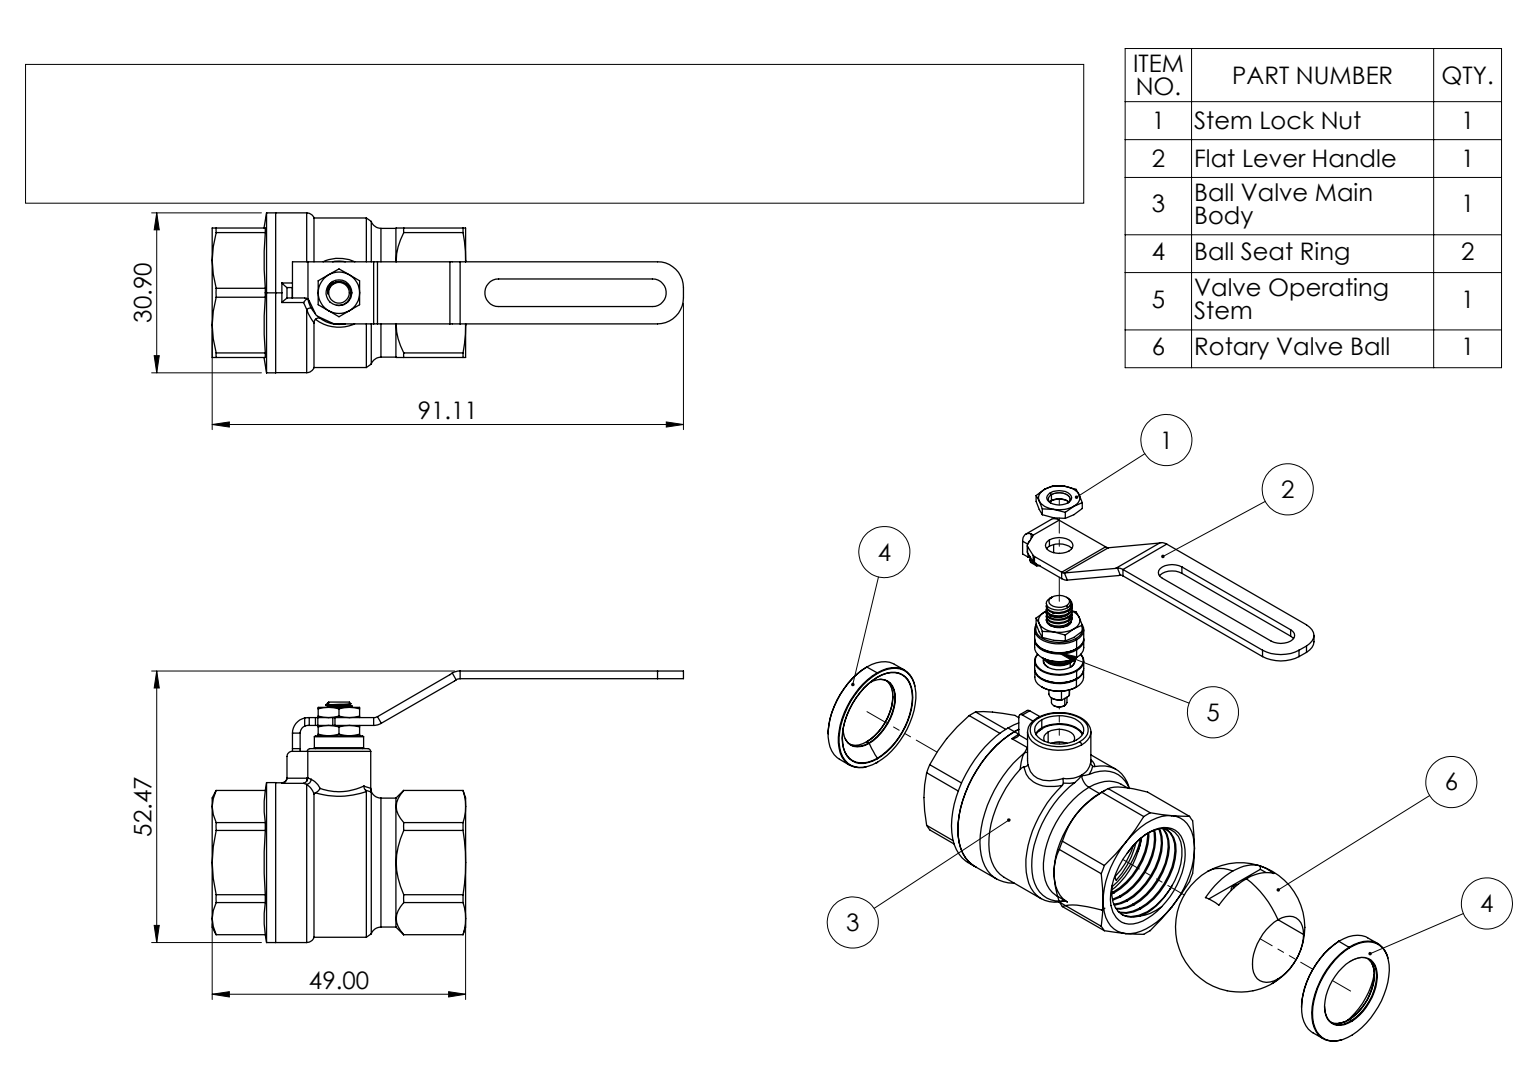
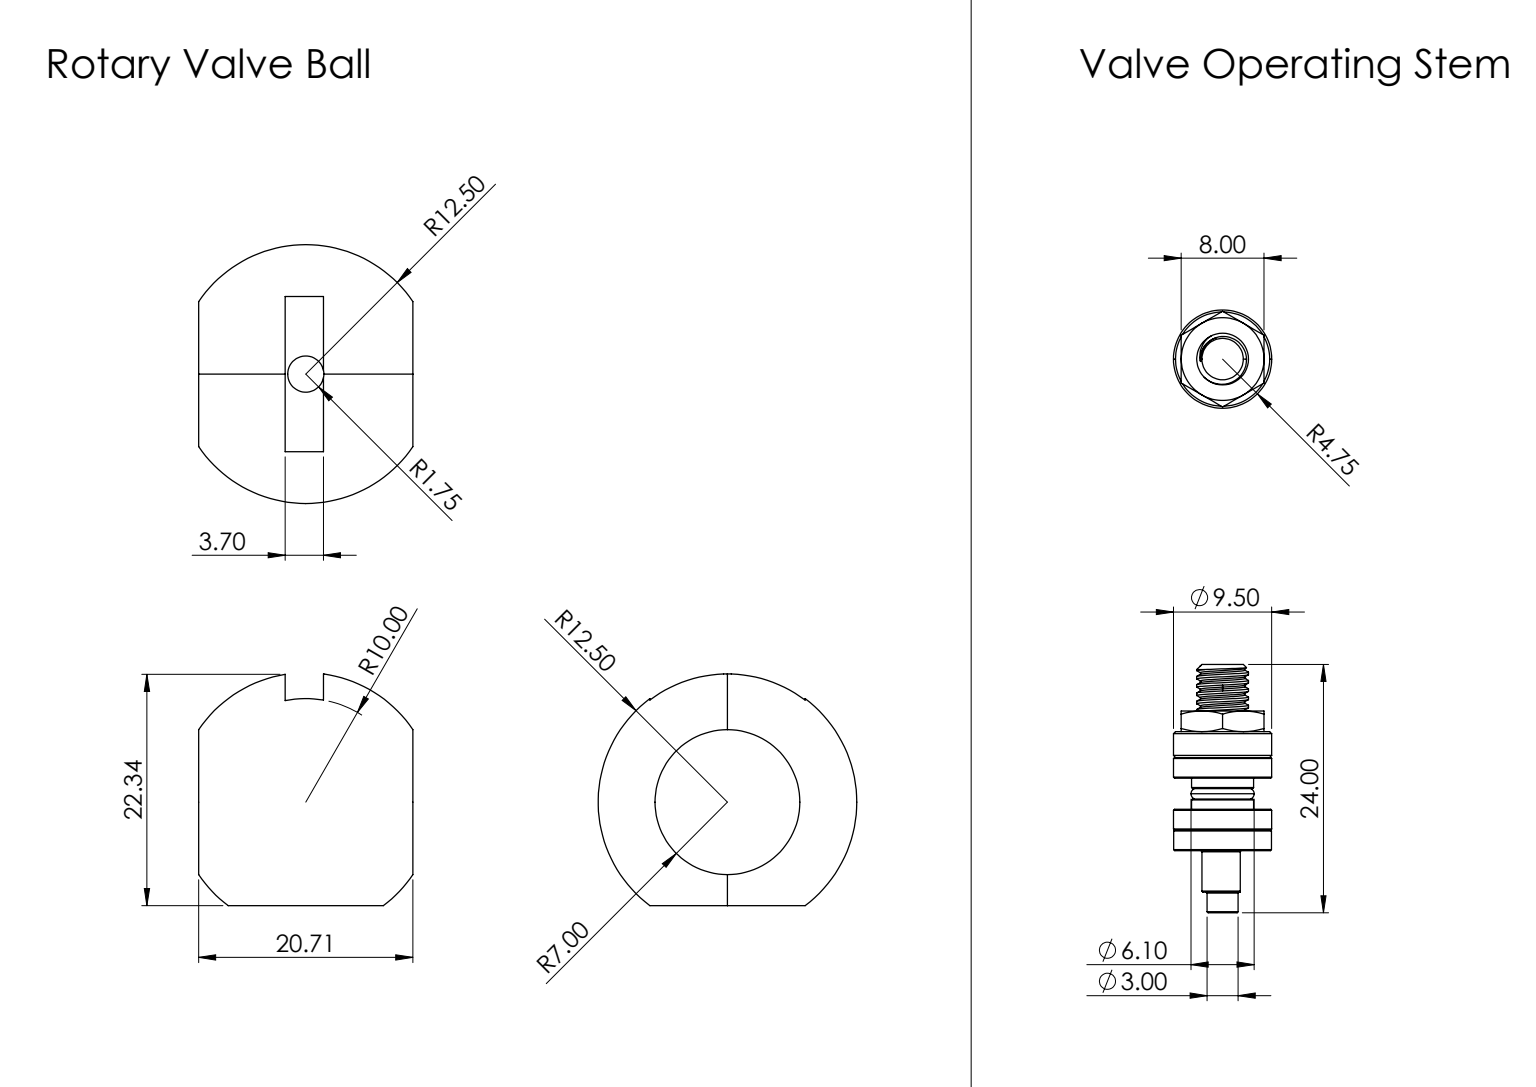
ISO-10303-21;
HEADER;
FILE_DESCRIPTION (('STEP AP214'),
    '1' );
FILE_NAME ('MAS-673',
    '2026-10-09T13:48:35',
    ( '' ),
    ( '' ),
    'SwSTEP 2.0',
    'SolidWorks 2026',
    '' );
FILE_SCHEMA (( 'AUTOMOTIVE_DESIGN' ));
ENDSEC;

DATA;
#1 = VERTEX_POINT ( 'NONE', #550 ) ;
#2 = CARTESIAN_POINT ( 'NONE',  ( -13.11728842303999976, -9.638936811879000643, -0.7309380707209000017 ) ) ;
#3 = CIRCLE ( 'NONE', #13143, 12.50000000000000178 ) ;
#4 = DIRECTION ( 'NONE',  ( 1.000000000000000000, 0.000000000000000000, 0.000000000000000000 ) ) ;
#5 = FACE_OUTER_BOUND ( 'NONE', #6433, .T. ) ;
#6 = EDGE_LOOP ( 'NONE', ( #5081, #3644, #13220, #12725 ) ) ;
#7 = CARTESIAN_POINT ( 'NONE',  ( -10.64042603139669296, 15.44559798911979875, -1.499885078173281761 ) ) ;
#8 = CARTESIAN_POINT ( 'NONE',  ( -1.666640107417000083, 24.57716808515000295, 1.349687702108000043 ) ) ;
#9 = CARTESIAN_POINT ( 'NONE',  ( 14.76827916823049058, 9.002773128276517767, -5.059891690319244795 ) ) ;
#10 = FACE_OUTER_BOUND ( 'NONE', #17299, .T. ) ;
#11 = CARTESIAN_POINT ( 'NONE',  ( 19.46336793902999673, -11.08665823510999893, -1.415474986610000041 ) ) ;
#12 = CARTESIAN_POINT ( 'NONE',  ( -0.8753480283797999695, 29.83343345458000329, -2.192249794771000015 ) ) ;
#13 = CARTESIAN_POINT ( 'NONE',  ( 14.10130024463479792, 4.527370814775449226, 7.815105637936889948 ) ) ;
#14 = CARTESIAN_POINT ( 'NONE',  ( -6.552349917305206439, 15.43140745850629436, -1.524086724148710381 ) ) ;
#15 = DIRECTION ( 'NONE',  ( 0.000000000000000000, 0.000000000000000000, 1.000000000000000000 ) ) ;
#16 = ADVANCED_FACE ( 'NONE', ( #18854 ), #20406, .T. ) ;
#17 = VERTEX_POINT ( 'NONE', #2260 ) ;
#18 = CARTESIAN_POINT ( 'NONE',  ( -2.277512614005948954, 24.29165256314995958, 1.108113113897667867 ) ) ;
#19 = CARTESIAN_POINT ( 'NONE',  ( 24.50000000000000355, -10.15196322910628446, 1.570734485538005432 ) ) ;
#20 = ORIENTED_EDGE ( 'NONE', *, *, #12798, .T. ) ;
#21 = CARTESIAN_POINT ( 'NONE',  ( 11.82354270082560532, -9.054930663370594601, -3.446502399965523988 ) ) ;
#22 = DIRECTION ( 'NONE',  ( -0.4719825803775118955, 0.1835218107899219686, 0.8622947226932178300 ) ) ;
#23 = CARTESIAN_POINT ( 'NONE',  ( 18.51344355829000321, 13.93375672974000068, 0.000000000000000000 ) ) ;
#24 = CARTESIAN_POINT ( 'NONE',  ( 19.10289643275000060, 0.6522580741204999644, 11.12207985314999803 ) ) ;
#25 = AXIS2_PLACEMENT_3D ( 'NONE', #17058, #6275, #4594 ) ;
#26 = CARTESIAN_POINT ( 'NONE',  ( -6.057596641756035183, 16.18429473919449890, 1.000000003976580842 ) ) ;
#27 = CARTESIAN_POINT ( 'NONE',  ( 1.652809762273000027, 26.39462896667000180, -2.096579189799000265 ) ) ;
#28 = EDGE_CURVE ( 'NONE', #3560, #10250, #9953, .T. ) ;
#29 = ORIENTED_EDGE ( 'NONE', *, *, #18417, .F. ) ;
#30 = CARTESIAN_POINT ( 'NONE',  ( -11.32728006584999925, -6.662114061867999482, 13.29187989938000136 ) ) ;
#31 = CARTESIAN_POINT ( 'NONE',  ( 0.000000000000000000, 28.00000000000000000, 0.000000000000000000 ) ) ;
#32 = DIRECTION ( 'NONE',  ( 0.000000000000000000, 0.000000000000000000, -1.000000000000000000 ) ) ;
#33 = ORIENTED_EDGE ( 'NONE', *, *, #678, .T. ) ;
#34 = CARTESIAN_POINT ( 'NONE',  ( -14.44097978627303469, 9.338505494776397242, 8.825220280766517433 ) ) ;
#35 = CARTESIAN_POINT ( 'NONE',  ( 18.85240113949000218, -1.886779804701000041, 10.26112574610000117 ) ) ;
#36 = B_SPLINE_CURVE_WITH_KNOTS ( 'NONE', 3,
 ( #18610, #11347, #22470, #18840, #2244, #6487, #13619, #2487, #661, #2741, #2366, #8067, #8431, #4429, #11583, #6112, #2611, #904 ),
 .UNSPECIFIED., .F., .F.,
 ( 4, 2, 2, 2, 2, 2, 2, 2, 4 ),
 ( 0.000000000000000000, 0.1250000000000000000, 0.2500000000000000000, 0.3750000000000000000, 0.5000000000000000000, 0.6250000000000000000, 0.7500000000000000000, 0.8750000000000000000, 1.000000000000000000 ),
 .UNSPECIFIED. ) ;
#37 = DIRECTION ( 'NONE',  ( 0.7071067811905932254, -0.7071067811824932603, 1.099460906822990477E-07 ) ) ;
#38 = CARTESIAN_POINT ( 'NONE',  ( 15.95305559329677436, -9.354823168593970451, -4.455688050559385438 ) ) ;
#39 = CARTESIAN_POINT ( 'NONE',  ( -16.96748435807999655, 1.976003357569000141, -10.89472041289000082 ) ) ;
#40 = CARTESIAN_POINT ( 'NONE',  ( -1.922540451232000125, 30.13691161737000002, -1.339163193283000153 ) ) ;
#41 = CARTESIAN_POINT ( 'NONE',  ( -14.13294016288999977, 9.260019365940999947, -2.871107829034000414 ) ) ;
#42 = EDGE_CURVE ( 'NONE', #6468, #23190, #12973, .T. ) ;
#43 = CARTESIAN_POINT ( 'NONE',  ( 2.033420667506555812, 29.75788411540394307, 0.7685308260835450600 ) ) ;
#44 = VERTEX_POINT ( 'NONE', #7955 ) ;
#45 = CARTESIAN_POINT ( 'NONE',  ( 0.5694918563224000696, 25.42220128840000015, 2.110394011463000208 ) ) ;
#46 = CARTESIAN_POINT ( 'NONE',  ( 19.50479438917271935, -10.32712268973978276, -1.911112615691448413 ) ) ;
#47 = CARTESIAN_POINT ( 'NONE',  ( -0.9075693228094323661, 23.65758229563746795, -1.957493242368112840 ) ) ;
#48 = ORIENTED_EDGE ( 'NONE', *, *, #10021, .F. ) ;
#49 = CARTESIAN_POINT ( 'NONE',  ( 4.864388344928220143, 14.50529179307395289, -3.789926123251598611 ) ) ;
#50 = EDGE_CURVE ( 'NONE', #3196, #1114, #6484, .T. ) ;
#51 = CARTESIAN_POINT ( 'NONE',  ( 11.28262625730999957, -8.806575700274999363, 0.9184129047361999643 ) ) ;
#52 = ORIENTED_EDGE ( 'NONE', *, *, #12758, .F. ) ;
#53 = B_SPLINE_CURVE_WITH_KNOTS ( 'NONE', 3,
 ( #23724, #16684, #11126, #22035, #20219, #20108, #94, #18511, #3517, #11252 ),
 .UNSPECIFIED., .F., .F.,
 ( 4, 2, 2, 2, 4 ),
 ( 0.000000000000000000, 0.1250000000000000000, 0.2500000000000000000, 0.4999999999999998890, 1.000000000000000000 ),
 .UNSPECIFIED. ) ;
#54 = CARTESIAN_POINT ( 'NONE',  ( -14.25243324638999809, 7.716878364870000340, -11.63397459621999985 ) ) ;
#55 = CARTESIAN_POINT ( 'NONE',  ( -1.999167105995447224, 29.68333333333333357, 1.536366799937292305 ) ) ;
#56 = ORIENTED_EDGE ( 'NONE', *, *, #14846, .T. ) ;
#57 = CARTESIAN_POINT ( 'NONE',  ( -15.49705420454666971, 1.186998013042136924, 9.068966667013654614 ) ) ;
#58 = CARTESIAN_POINT ( 'NONE',  ( 3.983126710162000705, 12.34486698612999866, 2.717232713520998377 ) ) ;
#59 = CARTESIAN_POINT ( 'NONE',  ( 12.00000000000000000, -1.960251216180438627, -9.262521325554040175 ) ) ;
#60 = CARTESIAN_POINT ( 'NONE',  ( -15.96442470609999909, 5.230920372153000208, -8.223195615302000050 ) ) ;
#61 = CARTESIAN_POINT ( 'NONE',  ( 18.86608333333332510, 2.396295210176243362, -8.917180031126768824 ) ) ;
#62 = CARTESIAN_POINT ( 'NONE',  ( -23.39238510356613077, -5.190431350648047726, 9.217397525632280875 ) ) ;
#63 = CARTESIAN_POINT ( 'NONE',  ( 2.213005609277820529, 26.38948373505501266, -0.6062005036607733821 ) ) ;
#64 = FACE_OUTER_BOUND ( 'NONE', #4786, .T. ) ;
#65 = CARTESIAN_POINT ( 'NONE',  ( -5.500092053744999099, 15.58942091952000020, 2.547331119493998042 ) ) ;
#66 = EDGE_CURVE ( 'NONE', #3183, #7147, #11899, .T. ) ;
#67 = CARTESIAN_POINT ( 'NONE',  ( 0.000000000000000000, 29.85000000000000142, 0.000000000000000000 ) ) ;
#68 = ORIENTED_EDGE ( 'NONE', *, *, #2410, .F. ) ;
#69 = ADVANCED_FACE ( 'NONE', ( #11713 ), #19084, .F. ) ;
#70 = CARTESIAN_POINT ( 'NONE',  ( 0.5551539414043799026, 26.26248452079970619, 2.089084675604010233 ) ) ;
#71 = CARTESIAN_POINT ( 'NONE',  ( 13.99789824808406102, 8.658198223038986896, -2.745508126827834516 ) ) ;
#72 = CARTESIAN_POINT ( 'NONE',  ( -22.78638441723432706, -9.917706536484757862, -3.646566398122319530 ) ) ;
#73 = CARTESIAN_POINT ( 'NONE',  ( 1.850881008969999852, 26.55271896306000201, 1.344743706340999934 ) ) ;
#74 = B_SPLINE_CURVE_WITH_KNOTS ( 'NONE', 3,
 ( #8588, #12348, #14154, #1319, #8708, #1438, #3264, #4839, #5196, #6638 ),
 .UNSPECIFIED., .F., .F.,
 ( 4, 2, 2, 2, 4 ),
 ( 0.000000000000000000, 0.1249999999999999722, 0.2499999999999999445, 0.4999999999999998890, 1.000000000000000000 ),
 .UNSPECIFIED. ) ;
#75 = CARTESIAN_POINT ( 'NONE',  ( -2.123790204974259410, 30.86901160495731133, 0.1750885401383986684 ) ) ;
#76 = CARTESIAN_POINT ( 'NONE',  ( 2.570568752299490445, 11.76159806634492000, 4.083892722200570091 ) ) ;
#77 = ORIENTED_EDGE ( 'NONE', *, *, #21426, .F. ) ;
#78 = CARTESIAN_POINT ( 'NONE',  ( -4.424293379393901660, 12.29270965195770771, -1.981197220050498808 ) ) ;
#79 = EDGE_CURVE ( 'NONE', #8805, #20876, #2608, .T. ) ;
#80 = CARTESIAN_POINT ( 'NONE',  ( 24.40278699097224901, 12.15528518867914620, 3.946428472716975833 ) ) ;
#81 = EDGE_CURVE ( 'NONE', #16646, #13895, #14967, .T. ) ;
#82 = DIRECTION ( 'NONE',  ( -1.000000000000000000, 0.000000000000000000, 0.000000000000000000 ) ) ;
#83 = ORIENTED_EDGE ( 'NONE', *, *, #21982, .F. ) ;
#84 = CARTESIAN_POINT ( 'NONE',  ( 0.000000000000000000, 22.00000000000000000, -2.704938617610999654E-14 ) ) ;
#85 = CARTESIAN_POINT ( 'NONE',  ( 15.06487658531000129, -2.993859790429000078, 9.737735315623000432 ) ) ;
#86 = CARTESIAN_POINT ( 'NONE',  ( 18.41753846593428889, 9.434636916628203807, -4.442455713531500372 ) ) ;
#87 = CARTESIAN_POINT ( 'NONE',  ( -1.259047450927242018, 29.16753006952333038, 2.184465970885648201 ) ) ;
#88 = CARTESIAN_POINT ( 'NONE',  ( -1.813125266397999980, 29.53638408233999968, 1.482067624179000065 ) ) ;
#89 = CARTESIAN_POINT ( 'NONE',  ( -5.194121241778000275, 0.000000000000000000, 0.000000000000000000 ) ) ;
#90 = CARTESIAN_POINT ( 'NONE',  ( 0.8889003272348959817, 24.49999999999999289, 2.308449506161659226 ) ) ;
#91 = VECTOR ( 'NONE', #21222, 1000.000000000000114 ) ;
#92 = B_SPLINE_CURVE_WITH_KNOTS ( 'NONE', 3,
 ( #2075, #11646, #16720, #15021, #5828, #18780, #22295, #18555, #5709, #11170 ),
 .UNSPECIFIED., .F., .F.,
 ( 4, 2, 2, 2, 4 ),
 ( 0.000000000000000000, 0.2500000000000000000, 0.5000000000000000000, 0.7500000000000000000, 1.000000000000000000 ),
 .UNSPECIFIED. ) ;
#93 = VERTEX_POINT ( 'NONE', #21155 ) ;
#94 = CARTESIAN_POINT ( 'NONE',  ( -24.37124162822892259, 12.10385983559126544, 4.035505227296849462 ) ) ;
#95 = CARTESIAN_POINT ( 'NONE',  ( 22.24919044816000024, 10.13534249229999951, 5.028067520505000054 ) ) ;
#96 = CARTESIAN_POINT ( 'NONE',  ( -24.02103270219855347, 2.506500440823137055, 9.528970304172808881 ) ) ;
#97 = ORIENTED_EDGE ( 'NONE', *, *, #6382, .F. ) ;
#98 = DIRECTION ( 'NONE',  ( 0.000000000000000000, 1.000000000000000000, 0.000000000000000000 ) ) ;
#99 = CARTESIAN_POINT ( 'NONE',  ( 24.00016455292000117, -9.066063387507998783, 2.014468017461000127 ) ) ;
#100 = CARTESIAN_POINT ( 'NONE',  ( -2.710948798071000088, 11.76207888428000103, 4.122880019904000548 ) ) ;
#101 = CARTESIAN_POINT ( 'NONE',  ( 1.956501129450092469, 29.05944223948321792, -0.9149880855959362513 ) ) ;
#102 = DIRECTION ( 'NONE',  ( 0.000000000000000000, 1.000000000000000000, 0.000000000000000000 ) ) ;
#103 = EDGE_LOOP ( 'NONE', ( #22830, #9902, #9803, #18093 ) ) ;
#104 = CARTESIAN_POINT ( 'NONE',  ( -0.8133812233904295086, 23.73829498092657531, 2.103014135165154563 ) ) ;
#105 = ORIENTED_EDGE ( 'NONE', *, *, #9875, .F. ) ;
#106 = CARTESIAN_POINT ( 'NONE',  ( 0.9654995472831999770, 25.19530436186999722, -2.146034520375999843 ) ) ;
#107 = CARTESIAN_POINT ( 'NONE',  ( 6.643062618671002006, 13.49901315086000686, 0.1224259533632999497 ) ) ;
#108 = CARTESIAN_POINT ( 'NONE',  ( -4.371488211232004595, 13.35998688340998619, 5.531286660341000250 ) ) ;
#109 = AXIS2_PLACEMENT_3D ( 'NONE', #17470, #8390, #618 ) ;
#110 = DIRECTION ( 'NONE',  ( 0.000000000000000000, -1.000000000000000000, 0.000000000000000000 ) ) ;
#111 = CARTESIAN_POINT ( 'NONE',  ( 0.000000000000000000, 19.04999994433000055, -2.949999944334000368 ) ) ;
#112 = CARTESIAN_POINT ( 'NONE',  ( 13.96800158531000058, -3.572926710108999870, -9.509691282521000488 ) ) ;
#113 = CARTESIAN_POINT ( 'NONE',  ( -12.30476703115999904, 8.600742661000001732, -2.211712587549000020 ) ) ;
#114 = CARTESIAN_POINT ( 'NONE',  ( 18.30262625730999915, -5.463569446885998993, 7.195226492777999638 ) ) ;
#115 = DIRECTION ( 'NONE',  ( 1.000000000000000000, 0.000000000000000000, 0.000000000000000000 ) ) ;
#116 = PRODUCT_DEFINITION ( 'UNKNOWN', '', #15975, #23669 ) ;
#117 = ORIENTED_EDGE ( 'NONE', *, *, #18565, .T. ) ;
#118 = CARTESIAN_POINT ( 'NONE',  ( -10.19274265977768579, 15.86535919139761219, -1.103256594710403160 ) ) ;
#119 = B_SPLINE_CURVE_WITH_KNOTS ( 'NONE', 3,
 ( #6295, #17317, #2307, #720, #6416, #11875, #4485, #2421, #8128, #2671, #16960, #10062, #17075, #17447, #15493, #7994, #19128, #22524, #22758, #5931, #9575, #4122, #840, #15126, #13437, #8242, #11756, #15368, #13799, #21198, #11640, #11519, #6177, #359, #18898, #13563, #9694, #473, #7877, #15244, #22636, #20957 ),
 .UNSPECIFIED., .F., .F.,
 ( 4, 2, 1, 2, 2, 2, 1, 2, 2, 2, 2, 2, 2, 2, 2, 1, 2, 2, 2, 1, 2, 2, 4 ),
 ( 0.000000000000000000, 0.06250000000000149880, 0.09375000000000216493, 0.1093750000000024009, 0.1250000000000026368, 0.1875000000000031641, 0.2187500000000033307, 0.2343750000000034139, 0.2500000000000034972, 0.3125000000000032752, 0.3750000000000030531, 0.5000000000000025535, 0.5625000000000022204, 0.6250000000000019984, 0.6875000000000016653, 0.7187500000000015543, 0.7343750000000015543, 0.7500000000000014433, 0.8125000000000007772, 0.8437500000000005551, 0.8593750000000005551, 0.8750000000000004441, 1.000000000000000000 ),
 .UNSPECIFIED. ) ;
#120 = CARTESIAN_POINT ( 'NONE',  ( 2.047900492968999675, 24.12888028435000010, -0.6367493590249000412 ) ) ;
#121 = CARTESIAN_POINT ( 'NONE',  ( 14.61520294907830220, 5.230627013449347551, -8.911388815577064193 ) ) ;
#122 = CARTESIAN_POINT ( 'NONE',  ( -2.000000000000000000, 18.27087121525220681, 0.000000000000000000 ) ) ;
#123 = CARTESIAN_POINT ( 'NONE',  ( 21.99610005449000028, 5.761042396082000749, -9.658588492111000789 ) ) ;
#124 = CARTESIAN_POINT ( 'NONE',  ( 0.4673507188188000261, 29.65618993841000162, -2.509968819301999776 ) ) ;
#125 = CARTESIAN_POINT ( 'NONE',  ( 14.19049813593658982, 1.989872659937805599, 8.829286609355607496 ) ) ;
#126 = CARTESIAN_POINT ( 'NONE',  ( -6.042815832213999983, 16.39253418350000047, -0.9999999878869999526 ) ) ;
#127 = DIRECTION ( 'NONE',  ( 0.000000000000000000, 1.000000000000000000, 0.000000000000000000 ) ) ;
#128 = CARTESIAN_POINT ( 'NONE',  ( 19.17264246499999913, -10.17294749490999983, 5.068503378665999648 ) ) ;
#129 = ORIENTED_EDGE ( 'NONE', *, *, #896, .T. ) ;
#130 = CONICAL_SURFACE ( 'NONE', #12534, 3.049999825846000157, 0.7853981633972997312 ) ;
#131 = CARTESIAN_POINT ( 'NONE',  ( -14.00000000000000000, -15.45000000000000107, 0.000000000000000000 ) ) ;
#132 = EDGE_LOOP ( 'NONE', ( #5049, #12022, #23215, #18123, #9264, #7095, #5187 ) ) ;
#133 = CARTESIAN_POINT ( 'NONE',  ( 0.000000000000000000, 24.50000000000000000, 0.000000000000000000 ) ) ;
#134 = CARTESIAN_POINT ( 'NONE',  ( -2.000000000000000000, 30.00000000000000000, -3.464101615137999968 ) ) ;
#135 = CARTESIAN_POINT ( 'NONE',  ( 14.44500238972999995, 0.2592567778176000370, -11.01108926215000139 ) ) ;
#136 = CARTESIAN_POINT ( 'NONE',  ( -5.833999999999999631, 1.296092693409999996E-14, 0.000000000000000000 ) ) ;
#137 = CARTESIAN_POINT ( 'NONE',  ( 0.5721489135196999865, 28.05212896667000066, -2.607696352436000176 ) ) ;
#138 = ORIENTED_EDGE ( 'NONE', *, *, #17688, .F. ) ;
#139 = ORIENTED_EDGE ( 'NONE', *, *, #19795, .T. ) ;
#140 = CARTESIAN_POINT ( 'NONE',  ( -11.21808363877000048, -14.99030728474000007, -2.625125111862999905 ) ) ;
#141 = CARTESIAN_POINT ( 'NONE',  ( -130.2348000000000070, 19.50000000000000000, -2.000000000000000000 ) ) ;
#142 = CARTESIAN_POINT ( 'NONE',  ( 0.1752525089982897022, 28.25094615491967787, -4.517620070270786492 ) ) ;
#143 = EDGE_CURVE ( 'NONE', #568, #7147, #7639, .T. ) ;
#144 = ORIENTED_EDGE ( 'NONE', *, *, #7334, .F. ) ;
#145 = CARTESIAN_POINT ( 'NONE',  ( -14.48875655809282925, 10.17731420664813413, 7.372365177881404996 ) ) ;
#146 = DIRECTION ( 'NONE',  ( 1.000000000000000000, 0.000000000000000000, 0.000000000000000000 ) ) ;
#147 = CARTESIAN_POINT ( 'NONE',  ( -12.25000000000000000, 1.374666032043000015E-14, 0.000000000000000000 ) ) ;
#148 = CARTESIAN_POINT ( 'NONE',  ( 15.93387064109369433, -9.634484427928969197, -3.804155515456032699 ) ) ;
#149 = CARTESIAN_POINT ( 'NONE',  ( -15.52217783781999927, -9.820682682945999886, -5.027779166633999708 ) ) ;
#150 = CARTESIAN_POINT ( 'NONE',  ( -0.8860051451328000427, 29.33568040543000066, 2.005734967351000098 ) ) ;
#151 = CIRCLE ( 'NONE', #16003, 10.59999999999999964 ) ;
#152 = CIRCLE ( 'NONE', #7126, 1.500000000000001332 ) ;
#153 = CARTESIAN_POINT ( 'NONE',  ( -13.60506528143999994, -10.72046298714999857, -0.8128029906560000351 ) ) ;
#154 = EDGE_CURVE ( 'NONE', #7280, #18990, #3410, .T. ) ;
#155 = CARTESIAN_POINT ( 'NONE',  ( 1.387834333747559601, 29.69250747415173919, 1.655459006554598878 ) ) ;
#156 = ORIENTED_EDGE ( 'NONE', *, *, #22236, .T. ) ;
#157 = CARTESIAN_POINT ( 'NONE',  ( -0.7494000042766999492, 23.97278996295999676, 2.212197947947999843 ) ) ;
#158 = CARTESIAN_POINT ( 'NONE',  ( 21.03695710696093002, -7.396588329481368795, 7.510079579479033818 ) ) ;
#159 = CARTESIAN_POINT ( 'NONE',  ( -18.65919487842199231, 9.743618663561477433, -3.843173192191704501 ) ) ;
#160 = EDGE_LOOP ( 'NONE', ( #4133, #21661, #12489 ) ) ;
#161 = CARTESIAN_POINT ( 'NONE',  ( 0.000000000000000000, 15.00000000000000000, 0.000000000000000000 ) ) ;
#162 = CARTESIAN_POINT ( 'NONE',  ( 1.633245533205915478, 30.34494809611083710, -1.942077254787831109 ) ) ;
#163 = CARTESIAN_POINT ( 'NONE',  ( -23.66121525787396962, 1.340508726618324875, -9.439414443187377657 ) ) ;
#164 = CARTESIAN_POINT ( 'NONE',  ( 17.78062642131000004, 8.824178357484999680, -4.146495103786000058 ) ) ;
#165 = VERTEX_POINT ( 'NONE', #14005 ) ;
#166 = CARTESIAN_POINT ( 'NONE',  ( 0.000000000000000000, 21.87500000000000000, 0.000000000000000000 ) ) ;
#167 = DIRECTION ( 'NONE',  ( 0.000000000000000000, -1.000000000000000000, 0.000000000000000000 ) ) ;
#168 = EDGE_CURVE ( 'NONE', #3985, #21240, #5700, .T. ) ;
#169 = ORIENTED_EDGE ( 'NONE', *, *, #6404, .T. ) ;
#170 = CARTESIAN_POINT ( 'NONE',  ( 23.00512270046333185, 8.092645076355477585, -4.664454223405380517 ) ) ;
#171 = CARTESIAN_POINT ( 'NONE',  ( -4.740217193165002563, 12.61471626404000013, 0.1260612930167998857 ) ) ;
#172 = CARTESIAN_POINT ( 'NONE',  ( -20.26299539000000038, -9.084714414767999457, 1.684552287285000061 ) ) ;
#173 = CARTESIAN_POINT ( 'NONE',  ( 19.11258103379665130, 1.199143088786357669, -9.161748211282004561 ) ) ;
#174 = CARTESIAN_POINT ( 'NONE',  ( -5.483292957314003679, 16.58400099841001918, -3.023963835265001343 ) ) ;
#175 = CARTESIAN_POINT ( 'NONE',  ( -20.53578614557788384, 8.740101311720026800, -5.830131322368356628 ) ) ;
#176 = CARTESIAN_POINT ( 'NONE',  ( 0.000000000000000000, 22.00000000000000000, 0.000000000000000000 ) ) ;
#177 = AXIS2_PLACEMENT_3D ( 'NONE', #2830, #2574, #6813 ) ;
#178 = DIRECTION ( 'NONE',  ( 0.000000000000000000, -1.000000000000000000, 0.000000000000000000 ) ) ;
#179 = CARTESIAN_POINT ( 'NONE',  ( -2.778011591584000239, 28.82750240009999843, -0.7249434865795999494 ) ) ;
#180 = EDGE_CURVE ( 'NONE', #2621, #20551, #276, .T. ) ;
#181 = CARTESIAN_POINT ( 'NONE',  ( 2.147278730106622735, 30.61751797242171591, -0.2331274669797682719 ) ) ;
#182 = EDGE_LOOP ( 'NONE', ( #11413, #48, #13723 ) ) ;
#183 = CARTESIAN_POINT ( 'NONE',  ( 18.24195353945000164, -4.137305632263999833, 8.809128702420998991 ) ) ;
#184 = CARTESIAN_POINT ( 'NONE',  ( 13.84234230361491136, 6.026165916141002832, -6.791106574337510970 ) ) ;
#185 = CARTESIAN_POINT ( 'NONE',  ( -23.10770091748028321, -7.661184619407800156, 7.290997633578977677 ) ) ;
#186 = CARTESIAN_POINT ( 'NONE',  ( 2.048219662131999907, 28.09696440325999944, -1.368576729846999962 ) ) ;
#187 = CARTESIAN_POINT ( 'NONE',  ( -2.123217625947178888, 30.87310701895514597, 0.1259251270839611692 ) ) ;
#188 = CARTESIAN_POINT ( 'NONE',  ( 1.053140587386698135, 11.53014013154227335, 4.696634005027855885 ) ) ;
#189 = ORIENTED_EDGE ( 'NONE', *, *, #3583, .F. ) ;
#190 = EDGE_CURVE ( 'NONE', #10715, #2693, #6863, .T. ) ;
#191 = CARTESIAN_POINT ( 'NONE',  ( -4.144738096053230514, 12.19662818091454426, -2.499798518877363485 ) ) ;
#192 = DIRECTION ( 'NONE',  ( -0.000000000000000000, -1.000000000000000000, -0.000000000000000000 ) ) ;
#193 = DIRECTION ( 'NONE',  ( 0.000000000000000000, 0.000000000000000000, -1.000000000000000000 ) ) ;
#194 = ORIENTED_EDGE ( 'NONE', *, *, #3061, .T. ) ;
#195 = EDGE_CURVE ( 'NONE', #7466, #23288, #17774, .T. ) ;
#196 = EDGE_CURVE ( 'NONE', #21988, #11568, #4015, .T. ) ;
#197 = DIRECTION ( 'NONE',  ( 0.000000000000000000, 1.000000000000000000, 0.000000000000000000 ) ) ;
#198 = CARTESIAN_POINT ( 'NONE',  ( 14.40675158531000122, 9.325397517960999139, -4.058504152148000088 ) ) ;
#199 = AXIS2_PLACEMENT_3D ( 'NONE', #21129, #11572, #17500 ) ;
#200 = CARTESIAN_POINT ( 'NONE',  ( -13.32870921828000021, 6.513713587124000171, -9.206748540250000445 ) ) ;
#201 = DIRECTION ( 'NONE',  ( 1.000000000000000000, 0.000000000000000000, 0.000000000000000000 ) ) ;
#202 = CARTESIAN_POINT ( 'NONE',  ( 16.54676537306000128, 2.042383563461999785, -10.64749026856999947 ) ) ;
#203 = CARTESIAN_POINT ( 'NONE',  ( 8.124934037954998800, 12.44999999999999929, 0.000000000000000000 ) ) ;
#204 = CIRCLE ( 'NONE', #7166, 10.59999999999999964 ) ;
#205 = ORIENTED_EDGE ( 'NONE', *, *, #8949, .F. ) ;
#206 = CARTESIAN_POINT ( 'NONE',  ( 1.709999999999999964, 9.000000000000000000, -7.500000000000000000 ) ) ;
#207 = CARTESIAN_POINT ( 'NONE',  ( 22.95738685678000124, -11.03983583171999960, 2.562588168388999943 ) ) ;
#208 = EDGE_CURVE ( 'NONE', #14474, #22330, #6328, .T. ) ;
#209 = DIRECTION ( 'NONE',  ( -1.000000000000000000, 0.000000000000000000, 0.000000000000000000 ) ) ;
#210 = ORIENTED_EDGE ( 'NONE', *, *, #15775, .T. ) ;
#211 = CARTESIAN_POINT ( 'NONE',  ( -12.48243343204000055, 6.965111533508000718, -5.686492047758000545 ) ) ;
#212 = CARTESIAN_POINT ( 'NONE',  ( 24.50000000000000000, -0.1464674377591403120, 10.48970002016351621 ) ) ;
#213 = CARTESIAN_POINT ( 'NONE',  ( -1.985161156765999468, 11.61875206719000175, 4.524354049390001187 ) ) ;
#214 = CARTESIAN_POINT ( 'NONE',  ( -0.8255343667490313564, 29.25365081292461511, -1.996006782196166229 ) ) ;
#215 = CARTESIAN_POINT ( 'NONE',  ( -21.47533412897999838, 2.576025989571999908, 10.78750342170000032 ) ) ;
#216 = ORIENTED_EDGE ( 'NONE', *, *, #13652, .F. ) ;
#217 = FACE_OUTER_BOUND ( 'NONE', #15939, .T. ) ;
#218 = ORIENTED_EDGE ( 'NONE', *, *, #9354, .F. ) ;
#219 = CARTESIAN_POINT ( 'NONE',  ( 1.782743705658000000, 25.02019945177000082, -1.221832406237000068 ) ) ;
#220 = CARTESIAN_POINT ( 'NONE',  ( 2.434931691670791931, 28.36666666666666359, 0.6543697108981911814 ) ) ;
#221 = FACE_OUTER_BOUND ( 'NONE', #22296, .T. ) ;
#222 = DIRECTION ( 'NONE',  ( -1.000000000000000000, 0.000000000000000000, 0.000000000000000000 ) ) ;
#223 = CIRCLE ( 'NONE', #13763, 3.100000000000000089 ) ;
#224 = CARTESIAN_POINT ( 'NONE',  ( 2.999999956181000016, 17.90000004382000043, -2.609181548331000199E-08 ) ) ;
#225 = FACE_OUTER_BOUND ( 'NONE', #6977, .T. ) ;
#226 = CARTESIAN_POINT ( 'NONE',  ( 17.17537674931000069, -4.906342569036000079, 9.567493125660998743 ) ) ;
#227 = CARTESIAN_POINT ( 'NONE',  ( -16.44889015301999891, 10.17473773424000072, -3.711315847300999948 ) ) ;
#228 = CIRCLE ( 'NONE', #16200, 9.999999999999996447 ) ;
#229 = DIRECTION ( 'NONE',  ( -0.5000000000000169864, 0.8660254037844288266, 0.000000000000000000 ) ) ;
#230 = ORIENTED_EDGE ( 'NONE', *, *, #502, .T. ) ;
#231 = CARTESIAN_POINT ( 'NONE',  ( -10.33759248878110526, 15.67666494535818345, -1.227313276238695794 ) ) ;
#232 = CARTESIAN_POINT ( 'NONE',  ( 0.02135780212313000137, 24.77319310863999746, -2.715970023235000141 ) ) ;
#233 = CARTESIAN_POINT ( 'NONE',  ( 13.88475961963752958, -9.356662177357431887, 4.335039568263141518 ) ) ;
#234 = CARTESIAN_POINT ( 'NONE',  ( 24.50000000000000000, -2.116736914405999759, 10.36413001332999961 ) ) ;
#235 = CARTESIAN_POINT ( 'NONE',  ( 23.83156968415000065, 6.491674009242999865, -9.245099637402999448 ) ) ;
#236 = CARTESIAN_POINT ( 'NONE',  ( 1.879564114486999893, 30.37427879440000211, -1.727888272304000106 ) ) ;
#237 = ADVANCED_FACE ( 'NONE', ( #3364 ), #23073, .T. ) ;
#238 = CARTESIAN_POINT ( 'NONE',  ( 14.09681483843687566, 4.646111251452054169, 7.745166602763706720 ) ) ;
#239 = CARTESIAN_POINT ( 'NONE',  ( 17.04048089729959514, -1.953626282727659813, 10.24653127456325130 ) ) ;
#240 = TOROIDAL_SURFACE ( 'NONE', #10710, 7.200000000000000178, 0.1000000000000000056 ) ;
#241 = FACE_OUTER_BOUND ( 'NONE', #11847, .T. ) ;
#242 = DIRECTION ( 'NONE',  ( 1.000000000000000000, 0.000000000000000000, 0.000000000000000000 ) ) ;
#243 = CARTESIAN_POINT ( 'NONE',  ( 20.33214806635999850, 10.44200582290999968, 4.567853760350999437 ) ) ;
#244 = ORIENTED_EDGE ( 'NONE', *, *, #16225, .T. ) ;
#245 = CARTESIAN_POINT ( 'NONE',  ( 11.78693030657509588, -12.98156941795602215, 2.515258941348812005 ) ) ;
#246 = ORIENTED_EDGE ( 'NONE', *, *, #14119, .T. ) ;
#247 = CARTESIAN_POINT ( 'NONE',  ( -15.91866243917330870, 4.572869834151166657, -7.933744804850305421 ) ) ;
#248 = CARTESIAN_POINT ( 'NONE',  ( 0.000000000000000000, 22.00000000000000000, -4.649999999999999467 ) ) ;
#249 = CARTESIAN_POINT ( 'NONE',  ( 0.1526552725783049125, 24.50000000000000000, 2.395140156181688074 ) ) ;
#250 = CARTESIAN_POINT ( 'NONE',  ( 14.80590418541999931, 10.54075670043000024, -3.228249601621000497 ) ) ;
#251 = CARTESIAN_POINT ( 'NONE',  ( 2.950000000000001954, 24.50000000000000000, 5.832343053588036738E-08 ) ) ;
#252 = CONICAL_SURFACE ( 'NONE', #13040, 1.949955127985000258, 0.7853751480324476786 ) ;
#253 = CARTESIAN_POINT ( 'NONE',  ( 1.182158213329999930, 28.43419433610000269, 2.320116128650000054 ) ) ;
#254 = EDGE_LOOP ( 'NONE', ( #5726, #17524, #14583, #2895 ) ) ;
#255 = ORIENTED_EDGE ( 'NONE', *, *, #14267, .T. ) ;
#256 = CARTESIAN_POINT ( 'NONE',  ( -0.3272492347489394104, 27.25086340285666253, -2.499999999999999112 ) ) ;
#257 = CARTESIAN_POINT ( 'NONE',  ( 1.660953982101407433, 6.978325578095221360, -0.5614028787491848194 ) ) ;
#258 = CARTESIAN_POINT ( 'NONE',  ( 17.75645603379667037, 9.126947370999710429, 1.332864221464923560 ) ) ;
#259 = VERTEX_POINT ( 'NONE', #12444 ) ;
#260 = CARTESIAN_POINT ( 'NONE',  ( 2.000000000000000000, 28.00000000000000000, -3.464101615137999968 ) ) ;
#261 = CARTESIAN_POINT ( 'NONE',  ( 20.92658103379664425, 1.205236576247646685, -9.208299026488377947 ) ) ;
#262 = LINE ( 'NONE', #11311, #3334 ) ;
#263 = CARTESIAN_POINT ( 'NONE',  ( 15.75513086676498808, -10.05562620695802778, 2.464334981930285995 ) ) ;
#264 = CARTESIAN_POINT ( 'NONE',  ( -15.91754618602999827, -1.832079236261000110, 10.89068162177000154 ) ) ;
#265 = CARTESIAN_POINT ( 'NONE',  ( 0.3255751167234999799, 29.40761742610999718, 2.168404648556000236 ) ) ;
#266 = AXIS2_PLACEMENT_3D ( 'NONE', #7745, #20699, #7979 ) ;
#267 = CARTESIAN_POINT ( 'NONE',  ( -19.46889333780000086, -9.261490887677000572, 5.613638565637999456 ) ) ;
#268 = CARTESIAN_POINT ( 'NONE',  ( 1.671545104861497988, 29.71636722689019194, 1.369186538342708204 ) ) ;
#269 = ORIENTED_EDGE ( 'NONE', *, *, #16936, .F. ) ;
#270 = CARTESIAN_POINT ( 'NONE',  ( 1.582682121269000097, 25.73607590313999793, 1.501367095590999901 ) ) ;
#271 = CARTESIAN_POINT ( 'NONE',  ( -2.153985071724999756, 30.83999999999999986, 0.1610847937796999751 ) ) ;
#272 = DIRECTION ( 'NONE',  ( -1.000000000000000000, 0.000000000000000000, 0.000000000000000000 ) ) ;
#273 =( REPRESENTATION_RELATIONSHIP ('NONE','NONE', #13682, #14475 ) REPRESENTATION_RELATIONSHIP_WITH_TRANSFORMATION ( #10971 )SHAPE_REPRESENTATION_RELATIONSHIP( ) );
#274 = EDGE_LOOP ( 'NONE', ( #645, #2365, #19266, #5031 ) ) ;
#275 = EDGE_CURVE ( 'NONE', #9922, #21280, #2869, .T. ) ;
#276 = CIRCLE ( 'NONE', #20030, 12.34057940292999511 ) ;
#277 = CARTESIAN_POINT ( 'NONE',  ( 24.32802197706151048, -3.549421024389301405, 12.49999999999999645 ) ) ;
#278 = FACE_OUTER_BOUND ( 'NONE', #7793, .T. ) ;
#279 = CARTESIAN_POINT ( 'NONE',  ( -23.58077218185689006, 2.644447661185095555, -9.069886164648769622 ) ) ;
#280 = CARTESIAN_POINT ( 'NONE',  ( 12.26981375731000057, 8.958847990383999260, 1.572873132563999965 ) ) ;
#281 = ORIENTED_EDGE ( 'NONE', *, *, #23157, .T. ) ;
#282 = AXIS2_PLACEMENT_3D ( 'NONE', #22952, #17521, #14002 ) ;
#283 = B_SPLINE_CURVE_WITH_KNOTS ( 'NONE', 3,
 ( #2361, #2125, #5763, #13373, #15188, #13148, #20776, #17138, #22466, #7940 ),
 .UNSPECIFIED., .F., .F.,
 ( 4, 2, 2, 2, 4 ),
 ( 0.000000000000000000, 0.2499999999999964473, 0.3749999999999970024, 0.4999999999999975575, 1.000000000000000000 ),
 .UNSPECIFIED. ) ;
#284 = CARTESIAN_POINT ( 'NONE',  ( -4.438477777721789863, 15.42756752407910170, 4.222605013734312962 ) ) ;
#285 = COLOUR_RGB ( '', 0.66274510, 0.83137255, 0.94901961) ;
#286 = CARTESIAN_POINT ( 'NONE',  ( 23.99062354302999722, -13.93375672974000068, 0.8660254037843999608 ) ) ;
#287 = B_SPLINE_SURFACE_WITH_KNOTS ( 'NONE', 3, 3, ( 
 ( #12787, #6851, #14366, #19939, #15924, #16045, #20175, #10379, #14247, #10738, #10621, #21642, #17769, #1171, #3238, #5058, #18007, #1411, #23683, #8804, #16167, #3360, #18130, #7091, #5283, #2110, #1762, #11084, #9619, #9270, #18702, #14817, #9500, #22568, #3935, #14710, #16527, #18818, #22211, #22102, #16753, #11212, #9151, #7435, #16875, #18469, #23914, #7324, #5512, #22329, #7684, #1881, #5625, #20640, #16645, #12890, #280, #20290, #5863, #4051, #5745, #15059, #18351, #3693, #3584, #22453, #51 ),
 ( #13008, #5975, #18592, #20409, #13136, #13247, #11444, #2226, #164, #1997, #20529, #3817, #13357, #17004, #9382, #403, #7801, #7555, #11329, #14934, #15173, #10967, #21248, #23041, #8411, #22801, #11922, #22682, #8040, #1007, #18941, #10222, #17238, #13482, #15649, #639, #19054, #2348, #6463, #15779, #9858, #766, #20884, #4291, #11800, #21120, #19177, #4660, #23168, #12046, #13845, #2586, #19430, #19307, #2840, #9738, #9975, #15289, #2719, #13722, #10101, #15414, #17365, #2467, #8286, #22920, #8166 ),
 ( #17489, #6588, #4531, #7922, #17123, #17614, #6218, #6090, #15534, #4407, #520, #13599, #883, #11680, #20997, #6339, #20758, #4167, #11563, #4900, #8648, #7383, #12288, #17738, #20238, #23287, #14092, #11146, #1143, #18531, #21487, #1260, #16012, #14765, #15895, #21365, #12843, #1940, #9328, #1703, #18413, #19677, #4781, #16702, #23406, #112, #6823, #14219, #3209, #6700, #2960, #3090, #12165, #9209, #5030, #10351, #13972, #19555, #9093, #12414, #10477, #16466, #21614, #10593, #3757, #11028, #1823 ),
 ( #19799, #5460, #17862, #17979, #8537, #23854, #7263, #14655, #22051, #16587, #3642, #23968, #22163, #5574, #12953, #20351, #11508, #7623, #226, #22508, #7862, #5918, #15355, #2526, #7983, #576, #13302, #17180, #6036, #22745, #20472, #20701, #2057, #22625, #460, #13424, #20582, #4110, #5809, #18996, #9681, #18882, #7747, #11627, #9447, #13191, #22273, #20824, #15230, #18650, #9797, #6161, #14999, #20944, #2291, #4234, #4349, #13546, #11740, #19114, #9562, #18759, #2406, #17062, #9918, #17304, #7499 ) ),
 .UNSPECIFIED., .F., .F., .F.,
 ( 4, 4 ),
 ( 4, 1, 1, 1, 1, 1, 1, 1, 1, 1, 1, 1, 1, 1, 1, 1, 1, 1, 1, 1, 1, 1, 1, 1, 1, 1, 1, 1, 1, 1, 1, 1, 1, 1, 1, 1, 1, 1, 1, 1, 1, 1, 1, 1, 1, 1, 1, 1, 1, 1, 1, 1, 1, 1, 1, 1, 1, 1, 1, 1, 1, 1, 1, 1, 4 ),
 ( -0.08331297109794000288, 1.083312971098000066 ),
 ( -0.02000000000000000042, -0.003749999999999999861, 0.01250000000000000069, 0.02875000000000000125, 0.04499999999999999833, 0.06124999999999999889, 0.07749999999999999944, 0.09375000000000000000, 0.1100000000000000006, 0.1262500000000000011, 0.1424999999999999878, 0.1587500000000000022, 0.1749999999999999889, 0.1912500000000000033, 0.2074999999999999900, 0.2237500000000000044, 0.2399999999999999911, 0.2562499999999999778, 0.2725000000000000200, 0.2887500000000000067, 0.3049999999999999933, 0.3212499999999999800, 0.3375000000000000222, 0.3537500000000000089, 0.3699999999999999956, 0.3862499999999999822, 0.4025000000000000244, 0.4187500000000000111, 0.4349999999999999978, 0.4512499999999999845, 0.4675000000000000266, 0.4837500000000000133, 0.5000000000000000000, 0.5162499999999999867, 0.5324999999999999734, 0.5487499999999999600, 0.5649999999999999467, 0.5812500000000000444, 0.5975000000000000311, 0.6137500000000000178, 0.6300000000000000044, 0.6462499999999999911, 0.6624999999999999778, 0.6787499999999999645, 0.6949999999999999512, 0.7112500000000000488, 0.7275000000000000355, 0.7437500000000000222, 0.7600000000000000089, 0.7762499999999999956, 0.7924999999999999822, 0.8087499999999999689, 0.8249999999999999556, 0.8412500000000000533, 0.8575000000000000400, 0.8737500000000000266, 0.8900000000000000133, 0.9062500000000000000, 0.9224999999999999867, 0.9387499999999999734, 0.9549999999999999600, 0.9712499999999999467, 0.9875000000000000444, 1.003749999999999920, 1.020000000000000018 ),
 .UNSPECIFIED. ) ;
#288 = ORIENTED_EDGE ( 'NONE', *, *, #9109, .T. ) ;
#289 = DIRECTION ( 'NONE',  ( 1.000000000000000000, 0.000000000000000000, 0.000000000000000000 ) ) ;
#290 = CARTESIAN_POINT ( 'NONE',  ( -23.29066724161056712, 1.115319073173602238, -9.351742763910808165 ) ) ;
#291 = CARTESIAN_POINT ( 'NONE',  ( -2.623770339515000050, 11.96261007116998876, 4.059183977495999684 ) ) ;
#292 = CARTESIAN_POINT ( 'NONE',  ( -21.81533334470000085, -7.216842995913999914, -6.341849293150000122 ) ) ;
#293 = CARTESIAN_POINT ( 'NONE',  ( -14.46758741243325375, 9.725949910464320780, -8.154098604241012183 ) ) ;
#294 = CARTESIAN_POINT ( 'NONE',  ( -9.481593150953709039E-06, 28.93474093911251899, 2.386566200631719870 ) ) ;
#295 = CARTESIAN_POINT ( 'NONE',  ( -3.025523437588010012, 26.41693820796410463, -2.872015382385962656 ) ) ;
#296 = CARTESIAN_POINT ( 'NONE',  ( -4.750000000000000000, 22.00000000000000000, 0.000000000000000000 ) ) ;
#297 = CARTESIAN_POINT ( 'NONE',  ( 2.155060826509969552, 30.59516583461061145, 0.1486681260086218093 ) ) ;
#298 = ORIENTED_EDGE ( 'NONE', *, *, #14807, .T. ) ;
#299 = CARTESIAN_POINT ( 'NONE',  ( 23.70554140955999856, 3.449944951013000249, 9.831907654028000820 ) ) ;
#300 = CARTESIAN_POINT ( 'NONE',  ( -3.800404330270033437, 13.28692498924355725, -5.638841271150126566 ) ) ;
#301 = FACE_BOUND ( 'NONE', #15644, .T. ) ;
#302 = CONICAL_SURFACE ( 'NONE', #14242, 13.23032192316000000, 1.235249617460683957 ) ;
#303 = ADVANCED_FACE ( 'NONE', ( #21762 ), #7109, .T. ) ;
#304 = CARTESIAN_POINT ( 'NONE',  ( -21.71532941640836256, 6.478598051102530953, 8.484119408269807039 ) ) ;
#305 = CARTESIAN_POINT ( 'NONE',  ( 2.462898805936000191, 27.21946440326000172, 0.04836512055251000058 ) ) ;
#306 = CARTESIAN_POINT ( 'NONE',  ( 24.50000000000000000, 9.974367097857467002, -1.221507673991182219E-15 ) ) ;
#307 = ORIENTED_EDGE ( 'NONE', *, *, #7999, .T. ) ;
#308 = CONICAL_SURFACE ( 'NONE', #4587, 4.649999883068000273, 0.7853981633972997312 ) ;
#309 = CARTESIAN_POINT ( 'NONE',  ( -18.57752051073732247, 7.457970117013407396, -7.338587964615391535 ) ) ;
#310 = CARTESIAN_POINT ( 'NONE',  ( 24.28255857085423131, 12.88093503250115290, 2.689566074712900434 ) ) ;
#311 = VECTOR ( 'NONE', #7009, 1000.000000000000000 ) ;
#312 = FACE_OUTER_BOUND ( 'NONE', #13683, .T. ) ;
#313 = ORIENTED_EDGE ( 'NONE', *, *, #11602, .F. ) ;
#314 = EDGE_CURVE ( 'NONE', #9720, #10966, #3257, .T. ) ;
#315 = CARTESIAN_POINT ( 'NONE',  ( 0.000000000000000000, 24.50000000000000000, 0.000000000000000000 ) ) ;
#316 = CIRCLE ( 'NONE', #702, 0.09999999999999939493 ) ;
#317 = CARTESIAN_POINT ( 'NONE',  ( 18.75768908530999823, -5.059016186635999723, 8.765201904772998986 ) ) ;
#318 = CARTESIAN_POINT ( 'NONE',  ( 23.15628936713000030, 9.265517736846000219, 0.000000000000000000 ) ) ;
#319 = LINE ( 'NONE', #2266, #19710 ) ;
#320 = CARTESIAN_POINT ( 'NONE',  ( 12.61921080085999947, 0.9513980104831999407, -10.33598124465999923 ) ) ;
#321 = DIRECTION ( 'NONE',  ( -0.5000000000000169864, 0.000000000000000000, 0.8660254037844289376 ) ) ;
#322 = ADVANCED_FACE ( 'NONE', ( #21399 ), #12199, .T. ) ;
#323 = DIRECTION ( 'NONE',  ( 0.000000000000000000, -5.996565258237000474E-10, 1.000000000000000000 ) ) ;
#324 = CARTESIAN_POINT ( 'NONE',  ( 23.85409420549000004, -5.578683381639000238, -8.657878734822000766 ) ) ;
#325 = AXIS2_PLACEMENT_3D ( 'NONE', #4418, #15903, #15423 ) ;
#326 = CARTESIAN_POINT ( 'NONE',  ( 23.99062354302999722, 13.93375672974000068, 0.8660254037843999608 ) ) ;
#327 = ORIENTED_EDGE ( 'NONE', *, *, #12498, .T. ) ;
#328 = CARTESIAN_POINT ( 'NONE',  ( 12.10126773346000029, 4.413167110502000945, -7.952200573155999486 ) ) ;
#329 = FACE_OUTER_BOUND ( 'NONE', #10599, .T. ) ;
#330 = CIRCLE ( 'NONE', #15027, 4.000000000000000000 ) ;
#331 = CARTESIAN_POINT ( 'NONE',  ( -4.229412747127002881, 12.27284885278998416, 2.242987681384999377 ) ) ;
#332 = CYLINDRICAL_SURFACE ( 'NONE', #6125, 2.649999999999999911 ) ;
#333 = EDGE_CURVE ( 'NONE', #8084, #19340, #13286, .T. ) ;
#334 = CARTESIAN_POINT ( 'NONE',  ( -19.61694117649999924, -4.574436835851999561, 10.04828037913000216 ) ) ;
#335 = ORIENTED_EDGE ( 'NONE', *, *, #11923, .F. ) ;
#336 = CLOSED_SHELL ( 'NONE', ( #19786, #22741, #8979, #14137, #5705, #10585, #19906, #17710, #15034, #14866, #16344, #2572, #1995, #20352, #20018, #16952, #22187, #19348, #3814, #13211, #2540, #15971, #923, #17120, #9106, #4929, #6763, #19413, #8384, #21247, #11430, #1672, #12020, #13623, #15533, #9283, #9847, #3649, #4205, #7320, #9527, #23189, #20165, #21835, #18823, #16204, #1398 ) ) ;
#337 = CARTESIAN_POINT ( 'NONE',  ( -2.102266727616999731, 23.66000000000000014, 0.4960590750638999569 ) ) ;
#338 = AXIS2_PLACEMENT_3D ( 'NONE', #14363, #14706, #10963 ) ;
#339 = ORIENTED_EDGE ( 'NONE', *, *, #9210, .F. ) ;
#340 = CARTESIAN_POINT ( 'NONE',  ( 5.083787571969999419, 13.95749297742998607, 4.279447512729996461 ) ) ;
#341 = CARTESIAN_POINT ( 'NONE',  ( -1.932944458086000017, 26.02049822780999833, -1.184521108792000010 ) ) ;
#342 = CARTESIAN_POINT ( 'NONE',  ( 16.76949770046334365, -9.101620074973595820, 1.191526229459673347 ) ) ;
#343 = FACE_OUTER_BOUND ( 'NONE', #17510, .T. ) ;
#344 = CARTESIAN_POINT ( 'NONE',  ( 0.000000000000000000, 24.50000000000000000, 0.000000000000000000 ) ) ;
#345 = CIRCLE ( 'NONE', #18552, 7.000000000000000000 ) ;
#346 = EDGE_CURVE ( 'NONE', #1455, #4875, #7182, .T. ) ;
#347 = CARTESIAN_POINT ( 'NONE',  ( -12.61636557635000067, 8.538192823868000048, -4.467067395255999607 ) ) ;
#348 = CONICAL_SURFACE ( 'NONE', #19319, 2.949999944334000368, 0.7853981633972997312 ) ;
#349 = DIRECTION ( 'NONE',  ( 1.000000000000000000, 0.000000000000000000, 0.000000000000000000 ) ) ;
#350 = VECTOR ( 'NONE', #9545, 1000.000000000000000 ) ;
#351 = CARTESIAN_POINT ( 'NONE',  ( -14.38789255204306983, 4.127795921197732198, 12.49979377836116967 ) ) ;
#352 = ORIENTED_EDGE ( 'NONE', *, *, #7893, .F. ) ;
#353 = CARTESIAN_POINT ( 'NONE',  ( 12.50448526289000029, -13.93375672974000068, -0.4329697263849999755 ) ) ;
#354 = CARTESIAN_POINT ( 'NONE',  ( -1.610156619168000125, 25.09339868065000090, 2.187314281954999995 ) ) ;
#355 = CARTESIAN_POINT ( 'NONE',  ( 13.81197141142692253, -8.026017885533216045, 6.503606596646131166 ) ) ;
#356 = CARTESIAN_POINT ( 'NONE',  ( -18.10467920454667023, 2.391415452762288396, -8.898052290273778198 ) ) ;
#357 = CARTESIAN_POINT ( 'NONE',  ( 22.21657238354000086, 10.93369321636999913, 2.658656121609999978 ) ) ;
#358 = CARTESIAN_POINT ( 'NONE',  ( 2.300563072390000130, 28.75630017058999854, 0.5287386102487999784 ) ) ;
#359 = CARTESIAN_POINT ( 'NONE',  ( 11.55284350193499421, 3.530773253024809044, 12.49989659317028057 ) ) ;
#360 = DIRECTION ( 'NONE',  ( 1.000000000000000000, 0.000000000000000000, 0.000000000000000000 ) ) ;
#361 = DIRECTION ( 'NONE',  ( -1.000000000000000000, 0.000000000000000000, 0.000000000000000000 ) ) ;
#362 = EDGE_CURVE ( 'NONE', #11065, #21095, #11524, .T. ) ;
#363 = CARTESIAN_POINT ( 'NONE',  ( 11.78924557931191508, 8.668821331434422461, -9.985146724201950263 ) ) ;
#364 = ORIENTED_EDGE ( 'NONE', *, *, #3722, .T. ) ;
#365 = ADVANCED_FACE ( 'NONE', ( #11334 ), #5191, .T. ) ;
#366 = CARTESIAN_POINT ( 'NONE',  ( 11.59051697473728915, -12.65550321738646211, 3.079847693958680743 ) ) ;
#367 = VERTEX_POINT ( 'NONE', #10972 ) ;
#368 = B_SPLINE_CURVE_WITH_KNOTS ( 'NONE', 3,
 ( #14625, #18275, #16435, #9625, #16880 ),
 .UNSPECIFIED., .F., .F.,
 ( 4, 1, 4 ),
 ( 0.000000000000000000, 0.5000000000000000000, 1.000000000000000000 ),
 .UNSPECIFIED. ) ;
#369 = CARTESIAN_POINT ( 'NONE',  ( -16.25878743917330738, -5.585226852001683895, -7.267873252428181274 ) ) ;
#370 = DIRECTION ( 'NONE',  ( -1.000000000000000000, 0.000000000000000000, 1.562509794170000285E-11 ) ) ;
#371 = PLANE ( 'NONE',  #4207 ) ;
#372 = B_SPLINE_CURVE_WITH_KNOTS ( 'NONE', 3,
 ( #3482, #1297, #5064, #12446, #15814 ),
 .UNSPECIFIED., .F., .F.,
 ( 4, 1, 4 ),
 ( 0.000000000000000000, 0.5000000000000000000, 1.000000000000000000 ),
 .UNSPECIFIED. ) ;
#373 = ORIENTED_EDGE ( 'NONE', *, *, #15908, .F. ) ;
#374 = CIRCLE ( 'NONE', #16631, 0.1000000000000004635 ) ;
#375 = CARTESIAN_POINT ( 'NONE',  ( 16.42996226602999954, 6.392378590226999613, -9.036000841113999371 ) ) ;
#376 = DIRECTION ( 'NONE',  ( 1.000000000000000000, 0.000000000000000000, 0.000000000000000000 ) ) ;
#377 = CARTESIAN_POINT ( 'NONE',  ( -1.864615697012000028, 27.26419433610000098, -2.183184479328999839 ) ) ;
#378 = ADVANCED_FACE ( 'NONE', ( #13011 ), #8274, .F. ) ;
#379 = VERTEX_POINT ( 'NONE', #22107 ) ;
#380 = ORIENTED_EDGE ( 'NONE', *, *, #4764, .F. ) ;
#381 = EDGE_CURVE ( 'NONE', #22357, #8048, #20063, .T. ) ;
#382 = CARTESIAN_POINT ( 'NONE',  ( -14.00000000000000355, -7.644428321857049013, -6.387186174123134386 ) ) ;
#383 = CARTESIAN_POINT ( 'NONE',  ( -10.90524221169000185, 10.44179980742999980, -11.54806271477999857 ) ) ;
#384 = DIRECTION ( 'NONE',  ( 0.000000000000000000, 1.000000000000000000, 0.000000000000000000 ) ) ;
#385 = FACE_OUTER_BOUND ( 'NONE', #7895, .T. ) ;
#386 = VERTEX_POINT ( 'NONE', #18474 ) ;
#387 = CARTESIAN_POINT ( 'NONE',  ( -20.45951251414000183, -9.400720611274998362, 2.131946015016999763 ) ) ;
#388 = CARTESIAN_POINT ( 'NONE',  ( -14.44633158889241287, 12.24656508597993465, 3.788310138426364215 ) ) ;
#389 = CARTESIAN_POINT ( 'NONE',  ( 6.192588632250580538, 13.91017593417528708, 0.8180097329473892120 ) ) ;
#390 = CARTESIAN_POINT ( 'NONE',  ( 15.71064099089155164, -9.557463844202629843, 3.988810051267251300 ) ) ;
#391 = CARTESIAN_POINT ( 'NONE',  ( -14.07687131757000110, -7.628531263931999540, 7.915986703987999640 ) ) ;
#392 = CARTESIAN_POINT ( 'NONE',  ( -2.192033073580000213, 29.19180636409000229, 0.05448754284059999231 ) ) ;
#393 = CARTESIAN_POINT ( 'NONE',  ( -15.83949910911000281, -2.044365629921999883, 10.61848174243000109 ) ) ;
#394 = CARTESIAN_POINT ( 'NONE',  ( 0.5586671089952324198, 29.63706544627255113, 2.086414242290000498 ) ) ;
#395 = ORIENTED_EDGE ( 'NONE', *, *, #16929, .T. ) ;
#396 = CARTESIAN_POINT ( 'NONE',  ( 0.3885665913385000225, 24.40991835864999970, -2.146603527457000116 ) ) ;
#397 = CARTESIAN_POINT ( 'NONE',  ( -4.649999999999999467, 15.00000000000000000, 0.000000000000000000 ) ) ;
#398 = CARTESIAN_POINT ( 'NONE',  ( 24.00016455292000117, 0.000000000000000000, 0.000000000000000000 ) ) ;
#399 = ORIENTED_EDGE ( 'NONE', *, *, #17076, .T. ) ;
#400 = CARTESIAN_POINT ( 'NONE',  ( -0.3006329639645716756, 24.53729095029033758, -2.348355141549282710 ) ) ;
#401 = CARTESIAN_POINT ( 'NONE',  ( -5.600650454439005443, 15.08708793369000034, 2.809640077540999759 ) ) ;
#402 = CARTESIAN_POINT ( 'NONE',  ( 0.000000000000000000, 19.09999999999999787, 0.000000000000000000 ) ) ;
#403 = CARTESIAN_POINT ( 'NONE',  ( 17.01281392131000203, -9.720744103539999514, -0.4165551917177999774 ) ) ;
#404 = ORIENTED_EDGE ( 'NONE', *, *, #21965, .F. ) ;
#405 = CARTESIAN_POINT ( 'NONE',  ( -6.303284018220003837, 15.85635455589998344, -1.061654000538000409 ) ) ;
#406 = DIRECTION ( 'NONE',  ( 0.000000000000000000, 1.000000000000000000, 0.000000000000000000 ) ) ;
#407 = ORIENTED_EDGE ( 'NONE', *, *, #646, .T. ) ;
#408 = CARTESIAN_POINT ( 'NONE',  ( -9.000000000000000000, 19.50000000000000000, -1.000000000000000000 ) ) ;
#409 = CARTESIAN_POINT ( 'NONE',  ( 21.43591666666666740, 2.413791263500860929, 8.981313434221711134 ) ) ;
#410 = CARTESIAN_POINT ( 'NONE',  ( 3.263729719675002361, 12.11073175708999017, 3.451513885400003367 ) ) ;
#411 = LINE ( 'NONE', #6349, #9892 ) ;
#412 = AXIS2_PLACEMENT_3D ( 'NONE', #8961, #23955, #5663 ) ;
#413 = CARTESIAN_POINT ( 'NONE',  ( 12.00000000000000355, -2.493385451254096719, -9.174917364955389232 ) ) ;
#414 = ORIENTED_CLOSED_SHELL ( 'NONE', *, #20462, .F. );
#415 = CARTESIAN_POINT ( 'NONE',  ( 0.000000000000000000, 20.00000000000000000, 0.000000000000000000 ) ) ;
#416 = CARTESIAN_POINT ( 'NONE',  ( -4.749997084077000054, 12.55000000011000161, -4.491085162427999259E-09 ) ) ;
#417 = DIRECTION ( 'NONE',  ( 0.000000000000000000, -0.8660254037844288266, -0.5000000000000169864 ) ) ;
#418 = SURFACE_STYLE_USAGE ( .BOTH. , #3952 ) ;
#419 = CARTESIAN_POINT ( 'NONE',  ( -0.6543697108982035049, 28.06753006952333962, -2.434931691670788823 ) ) ;
#420 = CARTESIAN_POINT ( 'NONE',  ( 2.138730754459550631, 30.58610565302236139, 0.3009471218714359630 ) ) ;
#421 = ORIENTED_EDGE ( 'NONE', *, *, #1138, .T. ) ;
#422 = CARTESIAN_POINT ( 'NONE',  ( 21.14071754283999738, 8.535971018086002005, -4.841000346350999628 ) ) ;
#423 = CARTESIAN_POINT ( 'NONE',  ( 2.342532432829844691, 12.98933061754887497, -6.293791080244014680 ) ) ;
#424 = CARTESIAN_POINT ( 'NONE',  ( 23.75352077758000036, 36.75000000000000000, 6.000000000000000000 ) ) ;
#425 = CARTESIAN_POINT ( 'NONE',  ( -23.56289929282874240, 7.339383936488848903, 7.628101533612420937 ) ) ;
#426 = CARTESIAN_POINT ( 'NONE',  ( 2.425010641684000046, 27.99946440325999930, 0.4330518317348999724 ) ) ;
#427 = CYLINDRICAL_SURFACE ( 'NONE', #12766, 2.999999999999999112 ) ;
#428 = ORIENTED_EDGE ( 'NONE', *, *, #18310, .F. ) ;
#429 = CARTESIAN_POINT ( 'NONE',  ( 0.000000000000000000, 13.04999996922999905, 0.000000000000000000 ) ) ;
#430 = CARTESIAN_POINT ( 'NONE',  ( -2.000000000000000000, 18.89999999999999858, -5.041390465489999878E-11 ) ) ;
#431 = DIRECTION ( 'NONE',  ( 0.000000000000000000, -1.000000000000000000, 0.000000000000000000 ) ) ;
#432 = DIRECTION ( 'NONE',  ( 1.000000000000000000, 0.000000000000000000, 0.000000000000000000 ) ) ;
#433 = ORIENTED_EDGE ( 'NONE', *, *, #18501, .F. ) ;
#434 = FACE_OUTER_BOUND ( 'NONE', #19147, .T. ) ;
#435 = CARTESIAN_POINT ( 'NONE',  ( 14.76225174930999984, 10.68374474379000105, -0.3265774252310000292 ) ) ;
#436 = EDGE_CURVE ( 'NONE', #17309, #8075, #16408, .T. ) ;
#437 = DIRECTION ( 'NONE',  ( 1.000000000000000000, 0.000000000000000000, 0.000000000000000000 ) ) ;
#438 = CARTESIAN_POINT ( 'NONE',  ( -14.25243324638999809, 13.93375672974000068, 0.8660254037843999608 ) ) ;
#439 = CARTESIAN_POINT ( 'NONE',  ( 17.96864037306000128, -10.01334466946000035, -4.258412611471999121 ) ) ;
#440 = CARTESIAN_POINT ( 'NONE',  ( -12.35833339120999952, 6.571898948015506114, -13.37941417155348311 ) ) ;
#441 = CARTESIAN_POINT ( 'NONE',  ( 2.500000000000000000, 29.43419673618999965, 0.000000000000000000 ) ) ;
#442 = CARTESIAN_POINT ( 'NONE',  ( 24.47949698200000057, 5.955140450698999999, -7.767301070824998988 ) ) ;
#443 = VECTOR ( 'NONE', #1417, 1000.000000000000000 ) ;
#444 = CARTESIAN_POINT ( 'NONE',  ( 3.025523437588010012, 29.91693820796410463, 2.872015382385962656 ) ) ;
#445 = ORIENTED_EDGE ( 'NONE', *, *, #2462, .F. ) ;
#446 = LINE ( 'NONE', #20929, #10787 ) ;
#447 = CARTESIAN_POINT ( 'NONE',  ( -2.183184479328999839, 27.17000240009999956, -1.864615697012000028 ) ) ;
#448 = CARTESIAN_POINT ( 'NONE',  ( -4.836833366243003418, 12.42306831226000874, 0.1266535678225001182 ) ) ;
#449 = CARTESIAN_POINT ( 'NONE',  ( 1.973182983453731110, 28.95032424988295361, 0.8828346089906928817 ) ) ;
#450 = ADVANCED_FACE ( 'NONE', ( #1885 ), #12791, .T. ) ;
#451 = CARTESIAN_POINT ( 'NONE',  ( -20.61944845118999936, 1.065297639031000054, -11.01620010679999950 ) ) ;
#452 = ORIENTED_EDGE ( 'NONE', *, *, #7334, .T. ) ;
#453 = DIRECTION ( 'NONE',  ( 0.000000000000000000, 0.000000000000000000, 1.000000000000000000 ) ) ;
#454 = CIRCLE ( 'NONE', #17487, 7.000000000000000000 ) ;
#455 = ORIENTED_EDGE ( 'NONE', *, *, #4994, .F. ) ;
#456 = DIRECTION ( 'NONE',  ( -0.000000000000000000, 1.000000000000000000, 0.000000000000000000 ) ) ;
#457 = CARTESIAN_POINT ( 'NONE',  ( 0.5071914623445000769, 28.61256359724000120, 2.254114612530000006 ) ) ;
#458 = FACE_OUTER_BOUND ( 'NONE', #14382, .T. ) ;
#459 = CARTESIAN_POINT ( 'NONE',  ( -1.433806482797786552, 6.927073644917858708, 1.013309697580697222 ) ) ;
#460 = CARTESIAN_POINT ( 'NONE',  ( 15.42037674930999991, -6.716928621565999791, 8.336789182003000676 ) ) ;
#461 = CARTESIAN_POINT ( 'NONE',  ( -19.53660345378999708, -7.531619525312000185, 7.381236299612999652 ) ) ;
#462 = CARTESIAN_POINT ( 'NONE',  ( 17.20575125731000199, -0.07625726307336000431, -9.225306777752001253 ) ) ;
#463 = CARTESIAN_POINT ( 'NONE',  ( -14.49454881829679920, -0.9069790025675873446, 12.49996723896235906 ) ) ;
#464 = EDGE_CURVE ( 'NONE', #9967, #1877, #3712, .T. ) ;
#465 = ORIENTED_EDGE ( 'NONE', *, *, #22112, .T. ) ;
#466 = FACE_OUTER_BOUND ( 'NONE', #8013, .T. ) ;
#467 = CARTESIAN_POINT ( 'NONE',  ( -2.300703130192000234, 23.53376433680000090, 1.041687086677999918 ) ) ;
#468 = CARTESIAN_POINT ( 'NONE',  ( 13.74204473073353938, -6.236800112200524993, 8.214069492593580435 ) ) ;
#469 = ORIENTED_EDGE ( 'NONE', *, *, #7744, .F. ) ;
#470 = DIRECTION ( 'NONE',  ( 0.000000000000000000, 1.000000000000000000, 0.000000000000000000 ) ) ;
#471 = CARTESIAN_POINT ( 'NONE',  ( 20.52772435074999891, 11.05526862676000022, 1.831395270467999881 ) ) ;
#472 = CARTESIAN_POINT ( 'NONE',  ( 0.2468081092584000213, 28.97172682739000038, -2.347611320519999545 ) ) ;
#473 = CARTESIAN_POINT ( 'NONE',  ( 11.83261479512707659, 4.444106517312727433, 12.50001436053427462 ) ) ;
#474 = CARTESIAN_POINT ( 'NONE',  ( 18.40646359464608395, 10.24499631306186309, 2.163839732140223848 ) ) ;
#475 = CARTESIAN_POINT ( 'NONE',  ( -4.394996721094583059, 13.55525068814215039, 5.016329272847380949 ) ) ;
#476 = CARTESIAN_POINT ( 'NONE',  ( -6.533908178998216520, 15.44339042599172096, 1.502435935679650614 ) ) ;
#477 = EDGE_CURVE ( 'NONE', #16405, #15685, #7206, .T. ) ;
#478 = CARTESIAN_POINT ( 'NONE',  ( -1.259047450927251788, 29.70086340285667603, -2.184465970885643316 ) ) ;
#479 = VERTEX_POINT ( 'NONE', #11804 ) ;
#480 = CIRCLE ( 'NONE', #22909, 2.000000000000000000 ) ;
#481 = CARTESIAN_POINT ( 'NONE',  ( 12.28779254561781720, -13.65788853942738079, 1.343868873886420845 ) ) ;
#482 = ORIENTED_EDGE ( 'NONE', *, *, #4216, .F. ) ;
#483 = PRODUCT ( 'Flat Lever Handle', 'Flat Lever Handle', '', ( #22105 ) ) ;
#484 = CARTESIAN_POINT ( 'NONE',  ( -2.453480368351999896, 24.91848166633000261, 1.213420540718000096 ) ) ;
#486 = CARTESIAN_POINT ( 'NONE',  ( 0.6591105980973780420, 24.04252312545441583, 2.091938566331359883 ) ) ;
#485 = DIRECTION ( 'NONE',  ( 0.000000000000000000, 0.000000000000000000, -1.000000000000000000 ) ) ;
#487 = CARTESIAN_POINT ( 'NONE',  ( 1.640193969998194001, 24.74015355458762144, 1.405240085690787843 ) ) ;
#488 = ORIENTED_EDGE ( 'NONE', *, *, #1439, .F. ) ;
#489 = CARTESIAN_POINT ( 'NONE',  ( -8.000000000000000000, 9.651424765286998664, 0.000000000000000000 ) ) ;
#490 = CARTESIAN_POINT ( 'NONE',  ( -6.161940360818770834, 15.88536285935762038, 1.094220165152027135 ) ) ;
#491 = EDGE_CURVE ( 'NONE', #13012, #9699, #7476, .T. ) ;
#492 = CARTESIAN_POINT ( 'NONE',  ( -1.955724675740084795, 26.26076676662178855, 0.9180910909140133080 ) ) ;
#493 = ORIENTED_EDGE ( 'NONE', *, *, #6761, .F. ) ;
#494 = EDGE_LOOP ( 'NONE', ( #4284, #23458, #17919 ) ) ;
#495 = CARTESIAN_POINT ( 'NONE',  ( -13.99999999999999822, -8.587304723161174991, -5.250545313949140258 ) ) ;
#496 = CARTESIAN_POINT ( 'NONE',  ( -11.00706471169000089, 4.728939151478000369, -14.83327577388999963 ) ) ;
#497 = CARTESIAN_POINT ( 'NONE',  ( 0.4206857880311101749, 6.789717089907916225, -1.702993728068331825 ) ) ;
#498 = CARTESIAN_POINT ( 'NONE',  ( 18.17812270046333367, -0.3397639754939833501, 9.228485993081845251 ) ) ;
#499 = EDGE_CURVE ( 'NONE', #17201, #19976, #8041, .T. ) ;
#500 = ORIENTED_EDGE ( 'NONE', *, *, #19755, .T. ) ;
#501 = CARTESIAN_POINT ( 'NONE',  ( -24.30210239110000003, -9.610041974782999930, 1.174637117329000002 ) ) ;
#502 = EDGE_CURVE ( 'NONE', #22896, #18160, #1313, .T. ) ;
#503 = CARTESIAN_POINT ( 'NONE',  ( -14.48092005499817247, 11.66846015894712707, 4.789644024569511771 ) ) ;
#504 = DIRECTION ( 'NONE',  ( 0.000000000000000000, -1.000000000000000000, 0.000000000000000000 ) ) ;
#505 = CARTESIAN_POINT ( 'NONE',  ( 15.77750233183371265, -10.22258791821789536, 1.644876861122036349 ) ) ;
#506 = CARTESIAN_POINT ( 'NONE',  ( -7.500000000000000000, 22.00000000000000000, 1.000000000000000000 ) ) ;
#507 = CARTESIAN_POINT ( 'NONE',  ( -0.7069816488115999720, 28.78845002726000146, 1.950778716412999936 ) ) ;
#508 = VECTOR ( 'NONE', #15268, 1000.000000000000000 ) ;
#509 = CARTESIAN_POINT ( 'NONE',  ( -13.40193493347000064, -7.644751109369999575, -7.551345029496000727 ) ) ;
#510 = CARTESIAN_POINT ( 'NONE',  ( 0.6475450134985413220, 29.64256677160481956, 2.060670777103924767 ) ) ;
#511 = EDGE_CURVE ( 'NONE', #20864, #19479, #19182, .T. ) ;
#512 = ORIENTED_EDGE ( 'NONE', *, *, #10459, .F. ) ;
#513 = CARTESIAN_POINT ( 'NONE',  ( 0.4803641815392999947, 23.81685268192000038, 2.132454625199999843 ) ) ;
#514 = EDGE_CURVE ( 'NONE', #17995, #19991, #13664, .T. ) ;
#515 = CARTESIAN_POINT ( 'NONE',  ( 0.000000000000000000, 26.50000000000000355, -2.399999999999955502 ) ) ;
#516 = ORIENTED_EDGE ( 'NONE', *, *, #16185, .F. ) ;
#517 = CARTESIAN_POINT ( 'NONE',  ( -22.26176253788000281, -9.242562415387000740, 0.000000000000000000 ) ) ;
#518 = CARTESIAN_POINT ( 'NONE',  ( -4.007822987411000959, 13.30559351321000783, 4.666582981500002170 ) ) ;
#519 = CARTESIAN_POINT ( 'NONE',  ( 0.000000000000000000, 18.00000000000000000, 0.000000000000000000 ) ) ;
#520 = CARTESIAN_POINT ( 'NONE',  ( 17.80706408530999951, 3.725969113535000155, -9.559170675091001712 ) ) ;
#521 = ORIENTED_EDGE ( 'NONE', *, *, #17867, .T. ) ;
#522 = CARTESIAN_POINT ( 'NONE',  ( -6.326119818082997170, 16.13697961988999552, -0.9718497405647000820 ) ) ;
#523 = CARTESIAN_POINT ( 'NONE',  ( 24.00034722001000276, 6.716786535997999685, 12.21137788282999992 ) ) ;
#524 = ORIENTED_EDGE ( 'NONE', *, *, #1140, .F. ) ;
#525 = DIRECTION ( 'NONE',  ( 0.000000000000000000, -0.9998947838056817528, -0.01450590632083973396 ) ) ;
#526 = CARTESIAN_POINT ( 'NONE',  ( 0.000000000000000000, 18.00000000000000000, 0.000000000000000000 ) ) ;
#527 = CARTESIAN_POINT ( 'NONE',  ( 3.924142709797999728, 12.31642185211999241, 2.670936164341001895 ) ) ;
#528 = CARTESIAN_POINT ( 'NONE',  ( -14.00000000000000000, -4.143720316427557115, 9.101378173059835319 ) ) ;
#529 = CARTESIAN_POINT ( 'NONE',  ( 18.34519826651710162, 8.005455623522196973, -6.676223990317056156 ) ) ;
#530 = CARTESIAN_POINT ( 'NONE',  ( 11.99999999999999822, 4.923960526494110646, -7.557474118975338051 ) ) ;
#531 = DIRECTION ( 'NONE',  ( 0.8660254037844288266, 0.5000000000000169864, 0.000000000000000000 ) ) ;
#532 = CARTESIAN_POINT ( 'NONE',  ( 22.24928936712999672, -9.242242329243000043, 0.000000000000000000 ) ) ;
#533 = CARTESIAN_POINT ( 'NONE',  ( -3.821520914465099672, 26.24995697614779644, -2.412446024836691461 ) ) ;
#534 = CARTESIAN_POINT ( 'NONE',  ( 0.000000000000000000, 26.20000000000000284, -4.618802153517000519 ) ) ;
#535 = CARTESIAN_POINT ( 'NONE',  ( -9.000000000000000000, 18.50000000000000000, -5.000000000000000000 ) ) ;
#536 = CARTESIAN_POINT ( 'NONE',  ( 0.3085936222218769731, 30.42196597467193087, 2.139114131937794205 ) ) ;
#537 = EDGE_CURVE ( 'NONE', #23889, #15891, #18705, .T. ) ;
#538 = ORIENTED_EDGE ( 'NONE', *, *, #15854, .F. ) ;
#539 = CARTESIAN_POINT ( 'NONE',  ( 23.65297967911999777, -3.219993159064999944, 9.343258505126000202 ) ) ;
#540 = CARTESIAN_POINT ( 'NONE',  ( 2.127428512114412751, 12.95714030754093926, -6.359730179768805947 ) ) ;
#541 = CARTESIAN_POINT ( 'NONE',  ( -23.65071241290791448, -9.336176072467093690, -1.519767395369341578 ) ) ;
#542 = CARTESIAN_POINT ( 'NONE',  ( -21.15302554097793575, -10.13353536419278278, 2.834801739046542757 ) ) ;
#543 = CARTESIAN_POINT ( 'NONE',  ( 0.4030006639746999686, 26.21114211382000292, 2.256729627096000002 ) ) ;
#544 = DIRECTION ( 'NONE',  ( 0.000000000000000000, -1.000000000000000000, 0.000000000000000000 ) ) ;
#545 = ORIENTED_EDGE ( 'NONE', *, *, #18849, .F. ) ;
#546 = CARTESIAN_POINT ( 'NONE',  ( -19.24739020423550073, -10.46819004694524757, -0.4592041673053260387 ) ) ;
#547 = CARTESIAN_POINT ( 'NONE',  ( -4.000000000000000000, 29.92936170367562809, -1.090349405812125694 ) ) ;
#548 = CIRCLE ( 'NONE', #19927, 0.09999999999999939493 ) ;
#549 = FACE_OUTER_BOUND ( 'NONE', #13999, .T. ) ;
#550 = CARTESIAN_POINT ( 'NONE',  ( -11.04281598264000053, 15.31903517167999951, 1.878299281558999834 ) ) ;
#551 = VERTEX_POINT ( 'NONE', #18822 ) ;
#552 = CARTESIAN_POINT ( 'NONE',  ( 4.000000000000000000, 29.81534065533123723, -1.802053058880664471 ) ) ;
#553 = CARTESIAN_POINT ( 'NONE',  ( 14.87193924930999955, 10.04572779547000039, 3.659788831486999960 ) ) ;
#554 = CARTESIAN_POINT ( 'NONE',  ( -14.14123061016000094, -9.145880708538998149, 6.639339533417000005 ) ) ;
#555 = DIRECTION ( 'NONE',  ( 1.000000000000000000, 0.000000000000000000, 0.000000000000000000 ) ) ;
#556 = CARTESIAN_POINT ( 'NONE',  ( 14.10926537306000128, -9.926075755316000837, 4.188684833930999218 ) ) ;
#557 = CARTESIAN_POINT ( 'NONE',  ( -1.783084334938916715, 30.87983632939971557, -1.147531989998553215 ) ) ;
#558 = DIRECTION ( 'NONE',  ( 0.000000000000000000, 1.000000000000000000, 0.000000000000000000 ) ) ;
#559 = CARTESIAN_POINT ( 'NONE',  ( 24.20819240979999876, 6.272633220716000046, -8.181320936509997921 ) ) ;
#560 = DIRECTION ( 'NONE',  ( 0.000000000000000000, 0.000000000000000000, -1.000000000000000000 ) ) ;
#561 = ORIENTED_EDGE ( 'NONE', *, *, #8358, .F. ) ;
#562 = CARTESIAN_POINT ( 'NONE',  ( 11.84472065189999945, 4.409932236062999777, -7.946371848247000713 ) ) ;
#563 = CARTESIAN_POINT ( 'NONE',  ( -1.394936847711000016, 28.62456776951999871, -2.276308483783000103 ) ) ;
#564 = AXIS2_PLACEMENT_3D ( 'NONE', #17689, #4734, #3281 ) ;
#565 = CARTESIAN_POINT ( 'NONE',  ( 3.627106408426999273, 12.14388422481000518, 3.038632416491001909 ) ) ;
#566 = CARTESIAN_POINT ( 'NONE',  ( 0.2179091018266194058, 28.81668098355705254, 2.159923230666197291 ) ) ;
#567 = CARTESIAN_POINT ( 'NONE',  ( -22.45737845476999794, 0.1502580860940999907, -11.11644552567000055 ) ) ;
#568 = VERTEX_POINT ( 'NONE', #9622 ) ;
#569 = CARTESIAN_POINT ( 'NONE',  ( -4.649999999999999467, 20.10000000000000142, 5.428583055299999740E-09 ) ) ;
#570 = EDGE_LOOP ( 'NONE', ( #6840, #10937, #15562, #10507 ) ) ;
#571 = ADVANCED_FACE ( 'NONE', ( #21002 ), #130, .F. ) ;
#572 = CARTESIAN_POINT ( 'NONE',  ( -24.33938584176924991, 2.815218398139987865, -12.49992678697366166 ) ) ;
#573 = CARTESIAN_POINT ( 'NONE',  ( 2.500000000000000000, 28.40000000000000213, 0.000000000000000000 ) ) ;
#574 = DIRECTION ( 'NONE',  ( 1.000000000000000000, 0.000000000000000000, 0.000000000000000000 ) ) ;
#575 = CARTESIAN_POINT ( 'NONE',  ( -0.3507184568084537046, 6.786897298932621503, 1.714069254809378551 ) ) ;
#576 = CARTESIAN_POINT ( 'NONE',  ( 16.40756424930999913, 8.766565845128001300, -6.190543086277999763 ) ) ;
#577 = CARTESIAN_POINT ( 'NONE',  ( -14.37682859208999986, 9.777980407524001549, -3.031781461267000211 ) ) ;
#578 = CIRCLE ( 'NONE', #21874, 4.625000000000000000 ) ;
#579 = B_SPLINE_CURVE_WITH_KNOTS ( 'NONE', 3,
 ( #6025, #20812, #13412, #20933 ),
 .UNSPECIFIED., .F., .F.,
 ( 4, 4 ),
 ( 0.000000000000000000, 0.6207796204815331231 ),
 .UNSPECIFIED. ) ;
#580 = CARTESIAN_POINT ( 'NONE',  ( 13.91512625730999986, 8.379890869990997970, -3.647050788746000194 ) ) ;
#581 = CARTESIAN_POINT ( 'NONE',  ( -14.48633704289819057, -1.427546401406459831, 12.50000676666411792 ) ) ;
#582 = ORIENTED_EDGE ( 'NONE', *, *, #5142, .F. ) ;
#583 = EDGE_CURVE ( 'NONE', #14220, #9013, #21124, .T. ) ;
#584 = DIRECTION ( 'NONE',  ( 0.000000000000000000, 1.000000000000000000, 0.000000000000000000 ) ) ;
#585 = CARTESIAN_POINT ( 'NONE',  ( 1.924317348631999991, 23.78992879440000152, 1.635700662827000107 ) ) ;
#586 = CARTESIAN_POINT ( 'NONE',  ( 4.418452478372458359, 14.62271791494141837, -4.243679542130283977 ) ) ;
#587 = EDGE_LOOP ( 'NONE', ( #22612, #16356, #15446, #22262 ) ) ;
#588 = CARTESIAN_POINT ( 'NONE',  ( 5.373625923053002573, 13.70222443717999816, -4.580663796643002605 ) ) ;
#589 = DIRECTION ( 'NONE',  ( -0.5000000000000169864, 0.8660254037844288266, 0.000000000000000000 ) ) ;
#590 = CARTESIAN_POINT ( 'NONE',  ( -5.529771451991000397, 1.198997689148999791E-14, 1.310996564781999865E-13 ) ) ;
#591 = CARTESIAN_POINT ( 'NONE',  ( 14.40647870685735832, -4.521102126905931939, 7.829235988601594975 ) ) ;
#592 = CARTESIAN_POINT ( 'NONE',  ( 17.90467403235581045, 0.4259370903896579907, -10.44751290468639660 ) ) ;
#593 = CARTESIAN_POINT ( 'NONE',  ( 2.399999999999999911, 30.00000000000000000, 0.000000000000000000 ) ) ;
#594 = B_SPLINE_CURVE_WITH_KNOTS ( 'NONE', 3,
 ( #15681, #11956, #10132, #23200, #19208, #22833, #547, #673, #21282, #4692 ),
 .UNSPECIFIED., .F., .F.,
 ( 4, 1, 1, 2, 2, 4 ),
 ( 0.000000000000000000, 0.2500000000000001110, 0.3750000000000002776, 0.4375000000000004441, 0.5000000000000005551, 1.000000000000000000 ),
 .UNSPECIFIED. ) ;
#595 =( NAMED_UNIT ( * ) SI_UNIT ( $, .STERADIAN. ) SOLID_ANGLE_UNIT ( ) );
#596 = B_SPLINE_CURVE_WITH_KNOTS ( 'NONE', 3,
 ( #7719, #3848, #14965, #1789 ),
 .UNSPECIFIED., .F., .F.,
 ( 4, 4 ),
 ( 0.000000000000000000, 1.000000000000000000 ),
 .UNSPECIFIED. ) ;
#597 = DIRECTION ( 'NONE',  ( 0.000000000000000000, -1.000000000000000000, 0.000000000000000000 ) ) ;
#598 = ORIENTED_EDGE ( 'NONE', *, *, #22681, .F. ) ;
#599 = AXIS2_PLACEMENT_3D ( 'NONE', #6456, #6583, #635 ) ;
#600 = CARTESIAN_POINT ( 'NONE',  ( 0.000000000000000000, 22.19999999999999574, 0.000000000000000000 ) ) ;
#601 = ORIENTED_EDGE ( 'NONE', *, *, #20949, .F. ) ;
#602 = EDGE_CURVE ( 'NONE', #12251, #21466, #20643, .T. ) ;
#603 = CARTESIAN_POINT ( 'NONE',  ( 2.457689475042000193, 26.10287641827000016, -0.8603483806163000347 ) ) ;
#605 = CARTESIAN_POINT ( 'NONE',  ( -24.50000000000000000, 1.721664336791999924E-14, 0.000000000000000000 ) ) ;
#604 = CARTESIAN_POINT ( 'NONE',  ( -4.270778468753240631, 12.23941797836552148, 2.280178412471628668 ) ) ;
#606 = DIRECTION ( 'NONE',  ( 0.000000000000000000, -1.000000000000000000, 0.000000000000000000 ) ) ;
#607 = CARTESIAN_POINT ( 'NONE',  ( 17.11793655645000101, 6.716980213484000650, 8.821080241391998200 ) ) ;
#608 = CARTESIAN_POINT ( 'NONE',  ( -20.82261444457166988, 6.350348985615495323, 6.750538350822437472 ) ) ;
#609 = CARTESIAN_POINT ( 'NONE',  ( 0.5047246425491000998, 25.99669433610000269, 2.826365205286999860 ) ) ;
#610 = ORIENTED_EDGE ( 'NONE', *, *, #17195, .T. ) ;
#611 = VERTEX_POINT ( 'NONE', #13485 ) ;
#612 = CARTESIAN_POINT ( 'NONE',  ( -14.00000000000000533, -1.777611135496285355, -9.431915595318816514 ) ) ;
#613 = DIRECTION ( 'NONE',  ( -1.000000000000000000, 0.000000000000000000, 0.000000000000000000 ) ) ;
#614 = CARTESIAN_POINT ( 'NONE',  ( -14.48875655809283103, -10.17731420665194797, -7.372365177876170073 ) ) ;
#615 = ORIENTED_EDGE ( 'NONE', *, *, #5201, .F. ) ;
#616 = ADVANCED_FACE ( 'NONE', ( #13361 ), #18050, .F. ) ;
#617 = CARTESIAN_POINT ( 'NONE',  ( -21.73160135699000151, 8.161745128470998978, -6.112658946955999539 ) ) ;
#618 = DIRECTION ( 'NONE',  ( 0.8571428571428744148, 0.000000000000000000, -0.5150787536376840725 ) ) ;
#619 = AXIS2_PLACEMENT_3D ( 'NONE', #16490, #18560, #23879 ) ;
#620 = DIRECTION ( 'NONE',  ( 0.000000000000000000, 1.000000000000000000, 0.000000000000000000 ) ) ;
#621 = CARTESIAN_POINT ( 'NONE',  ( 15.58141692657948596, -6.929050783388004398, 7.685657546460438638 ) ) ;
#622 = AXIS2_PLACEMENT_3D ( 'NONE', #21561, #12361, #8721 ) ;
#623 = CARTESIAN_POINT ( 'NONE',  ( -13.92238738939999898, -10.21016635782999948, -2.519686904309999864 ) ) ;
#624 = DIRECTION ( 'NONE',  ( 0.000000000000000000, 1.000000000000000000, 0.000000000000000000 ) ) ;
#625 = CARTESIAN_POINT ( 'NONE',  ( -21.05048866052816692, -7.545730853300948837, -7.331750953782708358 ) ) ;
#626 = CARTESIAN_POINT ( 'NONE',  ( -14.98621963600000129, -7.639996621784999498, -6.839520901588999280 ) ) ;
#627 = EDGE_CURVE ( 'NONE', #19479, #13618, #15418, .T. ) ;
#628 = CARTESIAN_POINT ( 'NONE',  ( 0.9831177708813756411, 29.66411096424411298, 1.923123576622347120 ) ) ;
#629 = VERTEX_POINT ( 'NONE', #20887 ) ;
#630 = AXIS2_PLACEMENT_3D ( 'NONE', #13866, #4916, #21270 ) ;
#631 = CARTESIAN_POINT ( 'NONE',  ( 1.951212462256999958, 24.89714145383999622, -1.307686770928999875 ) ) ;
#632 = DIRECTION ( 'NONE',  ( 1.000000000000000000, 0.000000000000000000, 0.000000000000000000 ) ) ;
#633 = ORIENTED_EDGE ( 'NONE', *, *, #7921, .T. ) ;
#634 = EDGE_CURVE ( 'NONE', #15280, #17036, #9741, .T. ) ;
#635 = DIRECTION ( 'NONE',  ( 0.000000000000000000, -0.8660254037844288266, 0.5000000000000169864 ) ) ;
#636 = CARTESIAN_POINT ( 'NONE',  ( -0.8571723963710232708, 30.47784972801583692, -2.388390780044352013 ) ) ;
#637 = CARTESIAN_POINT ( 'NONE',  ( 23.41677564524290744, 35.51856778792605240, -6.000000000000000000 ) ) ;
#638 = AXIS2_PLACEMENT_3D ( 'NONE', #10074, #6308, #11771 ) ;
#639 = CARTESIAN_POINT ( 'NONE',  ( 14.81906392131000061, -2.842327771818999871, 9.244929856806999524 ) ) ;
#640 = ORIENTED_EDGE ( 'NONE', *, *, #17076, .F. ) ;
#641 = CYLINDRICAL_SURFACE ( 'NONE', #10623, 1.000000000000000888 ) ;
#642 = B_SPLINE_CURVE_WITH_KNOTS ( 'NONE', 3,
 ( #11380, #22500, #11501, #18876 ),
 .UNSPECIFIED., .F., .F.,
 ( 4, 4 ),
 ( 0.000000000000000000, 1.000000000000000000 ),
 .UNSPECIFIED. ) ;
#643 = CARTESIAN_POINT ( 'NONE',  ( 21.34228936713000024, 9.218966921638999779, 0.000000000000000000 ) ) ;
#644 = CARTESIAN_POINT ( 'NONE',  ( -11.99999999434999864, -6.999999994347000154, -4.083277946868999946E-09 ) ) ;
#645 = ORIENTED_EDGE ( 'NONE', *, *, #11625, .F. ) ;
#646 = EDGE_CURVE ( 'NONE', #14845, #21017, #6325, .T. ) ;
#647 = CARTESIAN_POINT ( 'NONE',  ( -2.206474594537332301, 24.66792226721002734, 0.3902536378939148176 ) ) ;
#648 = CARTESIAN_POINT ( 'NONE',  ( 0.000000000000000000, 19.00000000000000000, 0.000000000000000000 ) ) ;
#649 = CARTESIAN_POINT ( 'NONE',  ( 24.29420393214009977, -1.914062225345805501, 10.44982418693062343 ) ) ;
#650 = DIRECTION ( 'NONE',  ( -1.000000000000000000, 0.000000000000000000, 0.000000000000000000 ) ) ;
#651 = CARTESIAN_POINT ( 'NONE',  ( 17.97914201263965595, -3.906812565131978499, -9.711116240607633898 ) ) ;
#652 = CARTESIAN_POINT ( 'NONE',  ( -23.74465998031000069, 6.216878364870000340, 12.50000000000000000 ) ) ;
#653 = CARTESIAN_POINT ( 'NONE',  ( 7.446152422707000618, 28.20096189432300093, 6.000000000000000000 ) ) ;
#654 = CARTESIAN_POINT ( 'NONE',  ( -4.094404611478998923, 14.04847595166999952, -4.434860849016999396 ) ) ;
#655 = CARTESIAN_POINT ( 'NONE',  ( -0.1784790855350541494, 26.24995697614779644, 4.515757205439222766 ) ) ;
#656 = AXIS2_PLACEMENT_3D ( 'NONE', #17617, #2470, #8045 ) ;
#657 = CARTESIAN_POINT ( 'NONE',  ( 4.829988586904999437, 14.79876397742000194, 3.766541904039999888 ) ) ;
#658 = LINE ( 'NONE', #11344, #22673 ) ;
#659 = CARTESIAN_POINT ( 'NONE',  ( 0.2265999339602371709, 30.41708343718551077, 2.150008283823798383 ) ) ;
#660 = ORIENTED_EDGE ( 'NONE', *, *, #21953, .T. ) ;
#661 = CARTESIAN_POINT ( 'NONE',  ( -17.01462077250666738, 1.192095737878705153, 9.107910416114240348 ) ) ;
#662 = CARTESIAN_POINT ( 'NONE',  ( 24.77691953824000137, -11.46202743651999967, -1.149253455826999781 ) ) ;
#663 = CARTESIAN_POINT ( 'NONE',  ( -2.692449147991668568, 13.04955071611749418, -6.167886193833035158 ) ) ;
#664 = DIRECTION ( 'NONE',  ( 0.000000000000000000, -1.000000000000000000, 0.000000000000000000 ) ) ;
#665 = ADVANCED_FACE ( 'NONE', ( #19057 ), #6222, .T. ) ;
#666 = CARTESIAN_POINT ( 'NONE',  ( -20.53716891550649493, 2.994023850388096708, -10.07133576860161739 ) ) ;
#667 = CARTESIAN_POINT ( 'NONE',  ( 1.525059720042999833, 26.53696440326000072, -1.934529033667000020 ) ) ;
#668 = EDGE_CURVE ( 'NONE', #9155, #14280, #5034, .T. ) ;
#669 = VECTOR ( 'NONE', #2870, 1000.000000000000000 ) ;
#670 = CARTESIAN_POINT ( 'NONE',  ( -3.316026328260925471, 24.63336607546987267, -2.704152903936609231 ) ) ;
#671 = ORIENTED_EDGE ( 'NONE', *, *, #1856, .T. ) ;
#672 = CARTESIAN_POINT ( 'NONE',  ( -17.65644968217466726, -7.789232886291271640, 6.951626983977684304 ) ) ;
#673 = CARTESIAN_POINT ( 'NONE',  ( -4.000000000000000000, 29.87418302490046784, -1.506880184559495239 ) ) ;
#674 = ADVANCED_BREP_SHAPE_REPRESENTATION ( '', ( #9053, #4390 ), #20254 ) ;
#675 = DIRECTION ( 'NONE',  ( -1.000000000000000000, 0.000000000000000000, 0.000000000000000000 ) ) ;
#676 = CARTESIAN_POINT ( 'NONE',  ( 0.000000000000000000, -1.100000000000000089, 0.000000000000000000 ) ) ;
#677 = ORIENTED_EDGE ( 'NONE', *, *, #17568, .T. ) ;
#678 = EDGE_CURVE ( 'NONE', #20171, #3348, #9524, .T. ) ;
#679 = CARTESIAN_POINT ( 'NONE',  ( 17.41195603379666323, 4.591934376281141539, -7.967326209410963145 ) ) ;
#680 = CARTESIAN_POINT ( 'NONE',  ( 15.63975174930999934, -10.61757272617999881, 1.417689269007999853 ) ) ;
#681 = CARTESIAN_POINT ( 'NONE',  ( -24.21952468797000080, 6.266457887630000556, -9.319163484501999051 ) ) ;
#682 = CARTESIAN_POINT ( 'NONE',  ( -17.18818582970000008, -2.107320772642000239, -11.18988855195000021 ) ) ;
#683 = FACE_OUTER_BOUND ( 'NONE', #12131, .T. ) ;
#684 = CARTESIAN_POINT ( 'NONE',  ( 15.05671080085999947, 8.813937669080001314, 7.134837867725000393 ) ) ;
#685 = PLANE ( 'NONE',  #6580 ) ;
#686 = AXIS2_PLACEMENT_3D ( 'NONE', #14903, #16842, #9819 ) ;
#687 = PLANE ( 'NONE',  #16444 ) ;
#688 = CARTESIAN_POINT ( 'NONE',  ( 22.17785865399000045, -8.361523973907999618, -4.965137225652999753 ) ) ;
#689 = PRODUCT_DEFINITION_SHAPE ( 'NONE', 'NONE',  #1482 ) ;
#690 = CARTESIAN_POINT ( 'NONE',  ( 3.999987874060709991, 24.60222989788993431, -1.328900689436832261 ) ) ;
#691 = EDGE_LOOP ( 'NONE', ( #20065, #169, #1554, #10397 ) ) ;
#692 = CARTESIAN_POINT ( 'NONE',  ( 4.829988586904999437, 14.79876397742000016, 3.766541904039999888 ) ) ;
#693 = CARTESIAN_POINT ( 'NONE',  ( 2.052373795670999979, 28.32413313894999973, -1.371352433351999744 ) ) ;
#694 = CARTESIAN_POINT ( 'NONE',  ( 4.543963002250998251, 12.38829681527001370, 1.501761386921000696 ) ) ;
#695 = CARTESIAN_POINT ( 'NONE',  ( 1.836104782222518272, 28.93328551889701927, 1.137863805830989783 ) ) ;
#696 = CARTESIAN_POINT ( 'NONE',  ( -22.95863209211000111, -11.00291023332999885, 1.684196372985999890 ) ) ;
#697 = ORIENTED_EDGE ( 'NONE', *, *, #21937, .T. ) ;
#698 = CARTESIAN_POINT ( 'NONE',  ( -1.600000000000000089, 9.000000000000000000, 0.000000000000000000 ) ) ;
#699 = ORIENTED_EDGE ( 'NONE', *, *, #1410, .F. ) ;
#700 = DIRECTION ( 'NONE',  ( -1.160410170730938003E-09, 2.689653288266210374E-16, -1.000000000000000000 ) ) ;
#701 = CARTESIAN_POINT ( 'NONE',  ( 4.835177208035999818, 0.000000000000000000, 0.000000000000000000 ) ) ;
#702 = AXIS2_PLACEMENT_3D ( 'NONE', #569, #19234, #6518 ) ;
#703 = CARTESIAN_POINT ( 'NONE',  ( 0.1193520287149335557, 6.778461007907296221, 1.747140996228561338 ) ) ;
#704 = CARTESIAN_POINT ( 'NONE',  ( -4.649999849441000421, 19.99999984944626874, 6.648422602291999773E-08 ) ) ;
#705 = CARTESIAN_POINT ( 'NONE',  ( -16.20500172382000059, 9.665285290698001575, -3.525418390172999850 ) ) ;
#706 = CARTESIAN_POINT ( 'NONE',  ( 16.54762625731000014, -6.940875756134999186, 6.051234330564000174 ) ) ;
#707 = CARTESIAN_POINT ( 'NONE',  ( -2.500000000000000000, 27.19999999999999929, 0.000000000000000000 ) ) ;
#708 = AXIS2_PLACEMENT_3D ( 'NONE', #10789, #16573, #20224 ) ;
#709 = VERTEX_POINT ( 'NONE', #2844 ) ;
#710 = CARTESIAN_POINT ( 'NONE',  ( 21.34228936713000024, 9.218966921638999779, 0.000000000000000000 ) ) ;
#711 = CARTESIAN_POINT ( 'NONE',  ( 0.2939441912399000101, 30.67376943012999746, 2.707931486699000079 ) ) ;
#712 = CARTESIAN_POINT ( 'NONE',  ( 0.6575429675851000022, 24.04609325200999947, -2.438473339150000196 ) ) ;
#713 = CIRCLE ( 'NONE', #14639, 1.600000000000000089 ) ;
#714 = CARTESIAN_POINT ( 'NONE',  ( 13.72851662033176545, -5.846715754974600721, 8.501542022457519110 ) ) ;
#715 = AXIS2_PLACEMENT_3D ( 'NONE', #6015, #15457, #201 ) ;
#716 = ORIENTED_EDGE ( 'NONE', *, *, #17809, .F. ) ;
#717 = CARTESIAN_POINT ( 'NONE',  ( 3.941498952056000871, 13.94384724320999602, -4.660668869226999078 ) ) ;
#718 = ADVANCED_FACE ( 'NONE', ( #10105 ), #8276, .T. ) ;
#719 = FACE_OUTER_BOUND ( 'NONE', #14130, .T. ) ;
#720 = CARTESIAN_POINT ( 'NONE',  ( 12.12543434885670557, -5.255139125142729739, 12.50003690309258353 ) ) ;
#721 = CARTESIAN_POINT ( 'NONE',  ( 17.15198968891989395, -5.679900478530641728, 8.758236662128663141 ) ) ;
#722 = PLANE ( 'NONE',  #6401 ) ;
#723 = VECTOR ( 'NONE', #21146, 1000.000000000000000 ) ;
#724 = DIRECTION ( 'NONE',  ( 0.000000000000000000, 1.000000000000000000, 0.000000000000000000 ) ) ;
#725 = CARTESIAN_POINT ( 'NONE',  ( 11.83261479512603032, 8.603276725239243916, -10.09871632138033881 ) ) ;
#726 = EDGE_LOOP ( 'NONE', ( #11462, #19788, #12642, #19276 ) ) ;
#727 = CARTESIAN_POINT ( 'NONE',  ( 11.43887872962553054, -12.36312605252038033, 3.586317572276362942 ) ) ;
#728 = ORIENTED_EDGE ( 'NONE', *, *, #1649, .T. ) ;
#729 = VECTOR ( 'NONE', #20922, 1000.000000000000000 ) ;
#730 = DIRECTION ( 'NONE',  ( 0.000000000000000000, 0.4098987730065234425, -0.9121310190360518710 ) ) ;
#732 = DIRECTION ( 'NONE',  ( 0.000000000000000000, -1.000000000000000000, 1.361873576874000145E-14 ) ) ;
#731 = CARTESIAN_POINT ( 'NONE',  ( -0.2205931549149543758, 11.48217017896666015, 4.812798745242788279 ) ) ;
#733 = CARTESIAN_POINT ( 'NONE',  ( 8.124934037954998800, 0.000000000000000000, 0.000000000000000000 ) ) ;
#734 = AXIS2_PLACEMENT_3D ( 'NONE', #10520, #4708, #10636 ) ;
#735 = CARTESIAN_POINT ( 'NONE',  ( 1.699986466736000068, 9.100024030970999434, -1.053574575520999757 ) ) ;
#736 = DIRECTION ( 'NONE',  ( 0.8660254037844288266, 0.5000000000000169864, 0.000000000000000000 ) ) ;
#737 = CARTESIAN_POINT ( 'NONE',  ( 2.844001364980000002, 26.19169433609999942, -0.3933730402103999824 ) ) ;
#738 = EDGE_LOOP ( 'NONE', ( #3127, #3699, #18368, #8559 ) ) ;
#739 = ORIENTED_EDGE ( 'NONE', *, *, #9983, .F. ) ;
#740 = CARTESIAN_POINT ( 'NONE',  ( -13.99999999999999645, -4.994886009442610408, -8.411685227471448201 ) ) ;
#741 = TOROIDAL_SURFACE ( 'NONE', #11184, 16.43375672870000059, 1.000000000000000000 ) ;
#742 = DIRECTION ( 'NONE',  ( 0.000000000000000000, 1.000000000000000000, 0.000000000000000000 ) ) ;
#743 = CARTESIAN_POINT ( 'NONE',  ( -24.24003052283108062, -9.030352382187791349, -9.358674018439064213 ) ) ;
#744 = VERTEX_POINT ( 'NONE', #12419 ) ;
#745 = CARTESIAN_POINT ( 'NONE',  ( -21.31634619217999926, 9.651037232871999549, -0.4757113999236000090 ) ) ;
#746 = CARTESIAN_POINT ( 'NONE',  ( -18.99854661335000117, -6.966878364870000340, 12.06698729810999993 ) ) ;
#747 = FACE_OUTER_BOUND ( 'NONE', #13182, .T. ) ;
#748 = CARTESIAN_POINT ( 'NONE',  ( 15.86493638691169750, -10.25014446212039587, -1.494075193881422514 ) ) ;
#749 = CARTESIAN_POINT ( 'NONE',  ( -17.80271749694000150, -11.00587167721000093, 1.406230294539999814 ) ) ;
#750 = CIRCLE ( 'NONE', #8500, 1.500000000000000000 ) ;
#751 = EDGE_CURVE ( 'NONE', #9876, #8499, #3436, .T. ) ;
#752 = CARTESIAN_POINT ( 'NONE',  ( 0.3930574723085999977, 29.80062481890999848, -2.323201669609999964 ) ) ;
#753 = CARTESIAN_POINT ( 'NONE',  ( -20.92181303178861285, -3.650616230715998611, -9.863665015250019152 ) ) ;
#754 = DIRECTION ( 'NONE',  ( 0.000000000000000000, 1.000000000000000000, 0.000000000000000000 ) ) ;
#755 = CARTESIAN_POINT ( 'NONE',  ( -1.524638832331740579, 29.50412033714126281, 1.529828458804661340 ) ) ;
#756 = ORIENTED_EDGE ( 'NONE', *, *, #12377, .F. ) ;
#757 = B_SPLINE_CURVE_WITH_KNOTS ( 'NONE', 3,
 ( #4909, #19684, #9987, #9865, #17250, #649, #2727, #21128, #10109, #8051, #22810, #15658, #13608, #11808, #19186, #17374, #14692, #12533, #7301, #12768, #5493, #20038, #5264, #1389, #17987, #1626, #9130, #19921, #10484, #3338, #5039, #10948, #22084, #10716, #12872, #20158, #3099, #3565, #8782, #16020, #18335, #1744, #16505, #18108, #23414, #3220, #14226, #23894, #12422, #17871, #23663, #1269, #8656, #5380, #23777, #14458, #7074, #9015, #6833, #21621, #19806, #1514, #10602, #16144, #6957, #23546, #14348, #8905, #21739, #5152, #21853, #7183, #16271, #12650, #3456, #10841, #18225, #16385, #14573, #21966, #20622, #6286, #7418, #14917, #3677, #22312, #833, #14800, #2661, #1860, #15603, #11310, #18451, #22436, #18799, #22871, #13669, #9482, #3918, #5846, #22196, #7666, #1979, #5728, #12990, #15040, #13115, #16858, #10055, #16987, #8120, #8235, #5609, #21063, #35 ),
 .UNSPECIFIED., .F., .F.,
 ( 4, 2, 2, 2, 2, 2, 1, 2, 2, 2, 2, 2, 2, 2, 2, 2, 2, 2, 2, 2, 2, 2, 2, 2, 2, 2, 2, 2, 2, 1, 2, 2, 2, 2, 2, 2, 2, 2, 2, 2, 2, 2, 2, 2, 2, 2, 2, 2, 2, 2, 2, 2, 1, 2, 2, 2, 2, 2, 4 ),
 ( 0.000000000000000000, 0.01562500000000001041, 0.03125000000000002082, 0.04687500000000002776, 0.06250000000000004163, 0.07812500000000005551, 0.09375000000000005551, 0.1093750000000000694, 0.1250000000000000833, 0.1406250000000000833, 0.1562500000000001110, 0.1718750000000001110, 0.1875000000000001110, 0.2031250000000001110, 0.2187500000000000833, 0.2343750000000000833, 0.2500000000000000555, 0.2656250000000000555, 0.2812500000000000555, 0.2968750000000001110, 0.3125000000000001110, 0.3281250000000001110, 0.3437500000000001110, 0.3593750000000001110, 0.3750000000000001110, 0.3906250000000001110, 0.4062500000000000555, 0.4375000000000000000, 0.4687500000000000000, 0.4999999999999999445, 0.5312499999999998890, 0.5624999999999998890, 0.5937499999999998890, 0.6093749999999998890, 0.6249999999999998890, 0.6406249999999998890, 0.6562499999999998890, 0.6718749999999998890, 0.6874999999999998890, 0.7031249999999998890, 0.7187499999999998890, 0.7343749999999998890, 0.7499999999999998890, 0.7656250000000000000, 0.7812500000000000000, 0.7968750000000000000, 0.8125000000000000000, 0.8281250000000000000, 0.8437500000000000000, 0.8593750000000000000, 0.8750000000000000000, 0.8906250000000000000, 0.9062500000000000000, 0.9218750000000001110, 0.9375000000000001110, 0.9531250000000001110, 0.9687500000000001110, 0.9843750000000001110, 1.000000000000000000 ),
 .UNSPECIFIED. ) ;
#758 = CARTESIAN_POINT ( 'NONE',  ( 1.561610636931999974, 24.12936603334999930, -1.754607357718999783 ) ) ;
#759 = CARTESIAN_POINT ( 'NONE',  ( -15.73633831973462627, -9.927802218130974410, -3.384033804227659648 ) ) ;
#760 = EDGE_LOOP ( 'NONE', ( #18118, #12193, #17888, #4633 ) ) ;
#761 = CARTESIAN_POINT ( 'NONE',  ( 2.063594504837999888E-14, 28.80370090847999975, 2.160000000000000142 ) ) ;
#762 = CARTESIAN_POINT ( 'NONE',  ( 5.670434974910000925, 13.86170818258000281, -2.692715480849998233 ) ) ;
#763 = EDGE_CURVE ( 'NONE', #9475, #2621, #228, .T. ) ;
#764 = CARTESIAN_POINT ( 'NONE',  ( -2.125680721937184270, 30.86389948294139174, 0.2107507025189759575 ) ) ;
#765 = CARTESIAN_POINT ( 'NONE',  ( -19.54076253787999562, 9.172736192578000214, 0.000000000000000000 ) ) ;
#766 = CARTESIAN_POINT ( 'NONE',  ( 14.16093892131000054, 8.852644193975999443, -3.852777470446999697 ) ) ;
#767 = ORIENTED_EDGE ( 'NONE', *, *, #4237, .F. ) ;
#768 = CARTESIAN_POINT ( 'NONE',  ( 18.55445603379666153, -8.961743277533855689, 2.117392749268326657 ) ) ;
#769 = CARTESIAN_POINT ( 'NONE',  ( 2.500000000000000000, 26.80000000000000071, 0.000000000000000000 ) ) ;
#770 = DIRECTION ( 'NONE',  ( -1.000000000000000000, 0.000000000000000000, 0.000000000000000000 ) ) ;
#771 = ORIENTED_EDGE ( 'NONE', *, *, #23253, .T. ) ;
#772 = FACE_OUTER_BOUND ( 'NONE', #7197, .T. ) ;
#773 = DIRECTION ( 'NONE',  ( 0.000000000000000000, -1.000000000000000000, 0.000000000000000000 ) ) ;
#774 = CARTESIAN_POINT ( 'NONE',  ( -23.47393953383764398, 4.611284423866098159, -8.094624080708051395 ) ) ;
#775 = LINE ( 'NONE', #13609, #20067 ) ;
#776 = CARTESIAN_POINT ( 'NONE',  ( 18.32399750313075515, 7.510740577353477221, -7.220990934370560943 ) ) ;
#777 = DIRECTION ( 'NONE',  ( 1.000000000000000000, 0.000000000000000000, 0.000000000000000000 ) ) ;
#778 = ADVANCED_FACE ( 'NONE', ( #10481 ), #23508, .F. ) ;
#779 = CARTESIAN_POINT ( 'NONE',  ( -14.49999965082560038, 10.56569440617048805, -6.699684590240016391 ) ) ;
#780 = CARTESIAN_POINT ( 'NONE',  ( 21.18914133790000065, -7.515829758343000044, -8.336216767992999266 ) ) ;
#781 = FACE_OUTER_BOUND ( 'NONE', #7651, .T. ) ;
#782 = CARTESIAN_POINT ( 'NONE',  ( 0.6543697108981985089, 28.80086340285667035, -2.434931691670790599 ) ) ;
#783 = DIRECTION ( 'NONE',  ( 0.5000000000000169864, 0.000000000000000000, -0.8660254037844289376 ) ) ;
#784 = CARTESIAN_POINT ( 'NONE',  ( -2.159368856259221925, 30.20672668618349732, 0.05129505110700336573 ) ) ;
#785 = ORIENTED_EDGE ( 'NONE', *, *, #1811, .T. ) ;
#786 = CARTESIAN_POINT ( 'NONE',  ( 23.19221516142773964, 4.107034334315931901, 8.330789669698718924 ) ) ;
#787 = CARTESIAN_POINT ( 'NONE',  ( 20.08633540235999959, 9.945159233172001123, 4.350446449599000509 ) ) ;
#788 = CARTESIAN_POINT ( 'NONE',  ( -2.719034288096889629, 13.05437085155837629, -6.157680525929839277 ) ) ;
#789 = FACE_OUTER_BOUND ( 'NONE', #3552, .T. ) ;
#790 = CARTESIAN_POINT ( 'NONE',  ( -20.10874691517809509, 10.28412968912246939, 2.114059615703416384 ) ) ;
#791 = CARTESIAN_POINT ( 'NONE',  ( -24.50000000000000000, -10.82531754731000007, -6.250000000000000000 ) ) ;
#792 = EDGE_CURVE ( 'NONE', #20057, #2983, #19245, .T. ) ;
#793 = FACE_OUTER_BOUND ( 'NONE', #14111, .T. ) ;
#794 = ORIENTED_EDGE ( 'NONE', *, *, #514, .F. ) ;
#795 = CARTESIAN_POINT ( 'NONE',  ( -16.95866875144658081, 1.228736841276851788, -10.34930314903842152 ) ) ;
#796 = LINE ( 'NONE', #15448, #669 ) ;
#797 = DIRECTION ( 'NONE',  ( -1.511005198495999796E-08, -0.9999999999999997780, -8.997177385936997916E-09 ) ) ;
#798 = AXIS2_PLACEMENT_3D ( 'NONE', #12824, #11004, #5550 ) ;
#799 = DIRECTION ( 'NONE',  ( 1.000000000000000000, 0.000000000000000000, 0.000000000000000000 ) ) ;
#800 = CARTESIAN_POINT ( 'NONE',  ( -14.09989322724901051, 9.032303263851988007, 3.309274488355915889E-05 ) ) ;
#801 = ORIENTED_EDGE ( 'NONE', *, *, #7489, .F. ) ;
#802 = CARTESIAN_POINT ( 'NONE',  ( 4.000000000000000000, 29.91693820796410108, -1.184172465503444904 ) ) ;
#803 = CARTESIAN_POINT ( 'NONE',  ( 13.33631424930999998, 2.709556187140999661, 10.30084784107000040 ) ) ;
#804 = CARTESIAN_POINT ( 'NONE',  ( -23.73776463305999940, 8.652042595619999332, 7.138803698541999587 ) ) ;
#805 = EDGE_CURVE ( 'NONE', #12931, #15294, #3214, .T. ) ;
#806 = CARTESIAN_POINT ( 'NONE',  ( -18.53906879230999749, -1.456153306622999910, 10.25029566457999941 ) ) ;
#807 = CARTESIAN_POINT ( 'NONE',  ( 19.16841666666666555, 8.924639406612350001, -2.398560541756590059 ) ) ;
#808 = EDGE_CURVE ( 'NONE', #11090, #23810, #13051, .T. ) ;
#809 = CARTESIAN_POINT ( 'NONE',  ( 16.27687451746000136, -4.819963443980000761, 8.480589539771001384 ) ) ;
#810 = DIRECTION ( 'NONE',  ( 0.000000000000000000, 0.000000000000000000, 1.000000000000000000 ) ) ;
#811 = CARTESIAN_POINT ( 'NONE',  ( -10.90000000000000036, -7.200000000000000178, -4.317526974828999792E-09 ) ) ;
#812 = CARTESIAN_POINT ( 'NONE',  ( 21.37540677533000277, -2.698669465534999645, 9.869515643728000498 ) ) ;
#813 = CYLINDRICAL_SURFACE ( 'NONE', #4199, 2.500000000000000000 ) ;
#814 = ORIENTED_EDGE ( 'NONE', *, *, #1841, .F. ) ;
#815 = DIRECTION ( 'NONE',  ( 0.000000000000000000, 1.000000000000000000, 0.000000000000000000 ) ) ;
#816 = CARTESIAN_POINT ( 'NONE',  ( 2.621867217767999581, 26.03250240010000027, 0.5899383557787000187 ) ) ;
#817 = CARTESIAN_POINT ( 'NONE',  ( 4.780913943838003277, 12.47998338134000029, -0.02289341065286999363 ) ) ;
#818 = CARTESIAN_POINT ( 'NONE',  ( 2.051290025358256663, 28.96319104023008251, 0.6762458295797231234 ) ) ;
#819 = CARTESIAN_POINT ( 'NONE',  ( -21.95612481742999833, 10.92660042548000021, 1.976132411670999955 ) ) ;
#820 = EDGE_CURVE ( 'NONE', #14252, #3985, #10762, .T. ) ;
#821 = ADVANCED_FACE ( 'NONE', ( #4665 ), #14975, .T. ) ;
#822 = CARTESIAN_POINT ( 'NONE',  ( -18.13088126894000141, 1.446686056264999920E-14, 0.000000000000000000 ) ) ;
#823 = ORIENTED_EDGE ( 'NONE', *, *, #5689, .F. ) ;
#824 = CARTESIAN_POINT ( 'NONE',  ( 2.749999993363999806, 22.20000000663619844, -7.185653629187000299E-09 ) ) ;
#825 = DIRECTION ( 'NONE',  ( 0.000000000000000000, -0.7071067811866525998, -0.7071067811864425456 ) ) ;
#826 = CARTESIAN_POINT ( 'NONE',  ( 0.3327206652627045513, 6.785866010577869645, 1.718147026174522196 ) ) ;
#827 = PLANE ( 'NONE',  #9206 ) ;
#828 = CARTESIAN_POINT ( 'NONE',  ( -17.09903927815000202, -2.106860712391000146, -11.18744719158000045 ) ) ;
#829 = CARTESIAN_POINT ( 'NONE',  ( 15.88950125731000007, 9.094565878156000593, 1.328064802524999921 ) ) ;
#830 = CARTESIAN_POINT ( 'NONE',  ( -1.536366799937282090, 27.31666666666666643, 1.999167105995454552 ) ) ;
#831 = VECTOR ( 'NONE', #22809, 1000.000000000000000 ) ;
#832 = ORIENTED_EDGE ( 'NONE', *, *, #21823, .T. ) ;
#833 = CARTESIAN_POINT ( 'NONE',  ( 20.11733268653172857, 10.39601757465827525, -1.570891001574004742 ) ) ;
#834 = CARTESIAN_POINT ( 'NONE',  ( -4.000000000000000888, 30.00000000000001066, 0.3708744353061897425 ) ) ;
#835 = CARTESIAN_POINT ( 'NONE',  ( 24.25008227645999881, 9.630770167580999797, -1.179429185905188964E-15 ) ) ;
#836 = CARTESIAN_POINT ( 'NONE',  ( 4.236807648326396780, 14.55040135328094664, -4.423799120031906007 ) ) ;
#837 = VERTEX_POINT ( 'NONE', #13850 ) ;
#838 = CARTESIAN_POINT ( 'NONE',  ( -3.719979053892001453, 14.47850010422000366, -4.885491426500000678 ) ) ;
#839 = CARTESIAN_POINT ( 'NONE',  ( 2.654275184457999703, 29.40713753664000052, -0.7025011426262000036 ) ) ;
#840 = CARTESIAN_POINT ( 'NONE',  ( 11.07373617191544568, 0.5001676860470258834, 12.49996440465858960 ) ) ;
#841 = CARTESIAN_POINT ( 'NONE',  ( 16.45505974129427784, 10.04716483004630589, -2.764689303999621650 ) ) ;
#842 = CARTESIAN_POINT ( 'NONE',  ( -15.61632910584000022, 9.072027496059000384, 0.000000000000000000 ) ) ;
#843 = DIRECTION ( 'NONE',  ( 0.000000000000000000, -0.8660254037844288266, 0.5000000000000169864 ) ) ;
#844 = CARTESIAN_POINT ( 'NONE',  ( 2.434931691670788823, 29.46753006952333465, -0.6543697108982007293 ) ) ;
#845 = ORIENTED_EDGE ( 'NONE', *, *, #12365, .T. ) ;
#846 = CARTESIAN_POINT ( 'NONE',  ( 0.000000000000000000, 16.94999982584599962, 0.000000000000000000 ) ) ;
#847 = CARTESIAN_POINT ( 'NONE',  ( 3.792011109391261403, 12.19794324411309105, -2.926137113678119128 ) ) ;
#848 = ORIENTED_EDGE ( 'NONE', *, *, #23627, .T. ) ;
#849 = CARTESIAN_POINT ( 'NONE',  ( -5.636695640436695243, 16.19553706042610841, -2.397992902333817344 ) ) ;
#850 = CARTESIAN_POINT ( 'NONE',  ( 1.259047450927267331, 28.50086340285666964, 2.184465970885634434 ) ) ;
#851 = CARTESIAN_POINT ( 'NONE',  ( -3.555098145900802198, 13.22760776865786170, 5.776756902176543917 ) ) ;
#852 = CIRCLE ( 'NONE', #19843, 3.000000000000000000 ) ;
#853 = CARTESIAN_POINT ( 'NONE',  ( 6.145626734707911432, 14.16193665001459223, -0.1742073854001389144 ) ) ;
#854 = CARTESIAN_POINT ( 'NONE',  ( -19.54076253787999562, 9.172736192578000214, 0.000000000000000000 ) ) ;
#855 = ORIENTED_CLOSED_SHELL ( 'NONE', *, #19304, .F. );
#856 = CARTESIAN_POINT ( 'NONE',  ( -0.7249434865795999494, 25.60669433610000212, -2.778011591584000239 ) ) ;
#857 = ORIENTED_EDGE ( 'NONE', *, *, #16914, .F. ) ;
#858 = ORIENTED_EDGE ( 'NONE', *, *, #6254, .F. ) ;
#859 = CARTESIAN_POINT ( 'NONE',  ( -13.99999999999999289, 1.810552339594545312, -9.225438086100725243 ) ) ;
#860 = CARTESIAN_POINT ( 'NONE',  ( -6.000000000000000000, 28.00000000000000000, 1.229194263906999929 ) ) ;
#861 = B_SPLINE_CURVE_WITH_KNOTS ( 'NONE', 3,
 ( #19771, #20125, #17948, #3533, #10915, #1353, #8744, #6919, #21705, #1597 ),
 .UNSPECIFIED., .F., .F.,
 ( 4, 1, 1, 2, 2, 4 ),
 ( 0.000000000000000000, 0.2500000000000001110, 0.3750000000000001665, 0.4375000000000002220, 0.5000000000000002220, 1.000000000000000000 ),
 .UNSPECIFIED. ) ;
#862 = CARTESIAN_POINT ( 'NONE',  ( -6.838539683295000060, 15.31903503039000114, -1.878299264234999821 ) ) ;
#863 = ORIENTED_EDGE ( 'NONE', *, *, #22126, .T. ) ;
#864 = CARTESIAN_POINT ( 'NONE',  ( 7.446152422707000618, 28.20096189432300093, -6.000000000000000000 ) ) ;
#865 = CARTESIAN_POINT ( 'NONE',  ( 6.227597389086636959, 13.75196057894610036, 1.343634751001441918 ) ) ;
#866 = CARTESIAN_POINT ( 'NONE',  ( 14.97278813112675167, 10.13360311651370615, 2.016797930637777458 ) ) ;
#867 = CARTESIAN_POINT ( 'NONE',  ( -19.42868733223000177, -9.644227811630997849, -5.575930749671000441 ) ) ;
#868 = CARTESIAN_POINT ( 'NONE',  ( 0.5078888037730999727, 28.64963248812999907, 2.300764967654999715 ) ) ;
#869 = CARTESIAN_POINT ( 'NONE',  ( -20.89607790604070914, -2.753905224125297480, -10.15048530611613664 ) ) ;
#870 = TOROIDAL_SURFACE ( 'NONE', #14801, 2.500000000000000000, 0.5500000000000000444 ) ;
#871 = CARTESIAN_POINT ( 'NONE',  ( -15.88025719033000094, -8.846829628555999747, 7.110504558004000053 ) ) ;
#872 = BREP_WITH_VOIDS ( 'NONE', #9631, ( #16413, #14644 ) );
#873 = CARTESIAN_POINT ( 'NONE',  ( -1.078583570490634580, 29.53717604031488264, 1.871305732765136121 ) ) ;
#874 = ORIENTED_EDGE ( 'NONE', *, *, #21732, .F. ) ;
#875 = CARTESIAN_POINT ( 'NONE',  ( -1.197401029466999889, 24.51483033690999846, 1.828754584808999883 ) ) ;
#876 = CARTESIAN_POINT ( 'NONE',  ( -16.72027023057977146, 10.39404030090816455, 0.6342462940522078929 ) ) ;
#877 = ORIENTED_EDGE ( 'NONE', *, *, #1121, .T. ) ;
#878 = LINE ( 'NONE', #6334, #10288 ) ;
#879 = CARTESIAN_POINT ( 'NONE',  ( 6.141155213800003843, 13.62012030888000069, -2.541026553239001284 ) ) ;
#880 = CARTESIAN_POINT ( 'NONE',  ( 12.00000000000000000, -1.561535578790016476, -8.842512525458630535 ) ) ;
#881 = LINE ( 'NONE', #11679, #5311 ) ;
#882 = EDGE_CURVE ( 'NONE', #17082, #17341, #6494, .T. ) ;
#883 = CARTESIAN_POINT ( 'NONE',  ( 17.58768908531000008, -3.881224882977999613, -9.490963515925001204 ) ) ;
#884 = ORIENTED_EDGE ( 'NONE', *, *, #314, .T. ) ;
#885 = CARTESIAN_POINT ( 'NONE',  ( -11.43647649291999890, 10.56401704806000019, 9.958020882561998022 ) ) ;
#886 = CARTESIAN_POINT ( 'NONE',  ( -14.25243324638999809, -6.216878364870000340, 12.50000000000000000 ) ) ;
#887 = DIRECTION ( 'NONE',  ( -1.000000000000000000, 0.000000000000000000, 0.000000000000000000 ) ) ;
#888 = PRODUCT_DEFINITION_SHAPE ( 'NONE', 'NONE',  #23975 ) ;
#889 = VERTEX_POINT ( 'NONE', #16732 ) ;
#890 = CARTESIAN_POINT ( 'NONE',  ( -3.000000000000000000, 23.00000000000000000, 0.000000000000000000 ) ) ;
#891 = CARTESIAN_POINT ( 'NONE',  ( 21.47370833333333096, 1.207328351017924462, 9.222339391325609981 ) ) ;
#892 = CARTESIAN_POINT ( 'NONE',  ( 0.000000000000000000, 24.50000000000000000, 0.000000000000000000 ) ) ;
#893 = CARTESIAN_POINT ( 'NONE',  ( -14.00000000000000000, -5.950771400213850093, 8.190499872437872142 ) ) ;
#894 = CARTESIAN_POINT ( 'NONE',  ( 18.38411873406448294, 8.826705673792748286, -5.540809837595687348 ) ) ;
#895 = CARTESIAN_POINT ( 'NONE',  ( -6.250000012226999857, 15.73199627394999922, 1.185103398761000015 ) ) ;
#896 = EDGE_CURVE ( 'NONE', #16467, #5788, #1395, .T. ) ;
#897 = FACE_OUTER_BOUND ( 'NONE', #22469, .T. ) ;
#898 = CARTESIAN_POINT ( 'NONE',  ( 24.08896737927999965, 6.587527820344000418, 9.185660392408999897 ) ) ;
#899 = CARTESIAN_POINT ( 'NONE',  ( -0.7318187998270080374, 26.37490599056236817, 4.196286372439437251 ) ) ;
#900 = CARTESIAN_POINT ( 'NONE',  ( -3.861659623566732424, 14.00549260456081058, -4.847283716246065133 ) ) ;
#901 = DIRECTION ( 'NONE',  ( 0.000000000000000000, 0.000000000000000000, -1.000000000000000000 ) ) ;
#902 = CARTESIAN_POINT ( 'NONE',  ( -2.152354865182170673, 30.19285038283803502, -0.1835425803383945731 ) ) ;
#903 = VERTEX_POINT ( 'NONE', #1855 ) ;
#904 = CARTESIAN_POINT ( 'NONE',  ( -16.52332910583999848, -9.095302903661998783, 0.000000000000000000 ) ) ;
#905 = CARTESIAN_POINT ( 'NONE',  ( 21.63234287083999874, 9.479527916586000913, -5.375967906524000028 ) ) ;
#906 = CARTESIAN_POINT ( 'NONE',  ( 23.33520118364659623, -6.718265184276733137, -8.198908078898558216 ) ) ;
#907 = CARTESIAN_POINT ( 'NONE',  ( -2.500000000000000444, 27.45086340285666537, 0.3272492347489422415 ) ) ;
#908 = CARTESIAN_POINT ( 'NONE',  ( 1.127279431983196911, 24.69814275126839576, 1.904603634755329900 ) ) ;
#909 = CARTESIAN_POINT ( 'NONE',  ( 4.852652572476451098, 14.56096245632547692, 3.781519854356791832 ) ) ;
#910 = CARTESIAN_POINT ( 'NONE',  ( -4.940724180147997302, 12.51283282727001556, 0.1567042536069999104 ) ) ;
#911 = ORIENTED_EDGE ( 'NONE', *, *, #23001, .F. ) ;
#912 = EDGE_CURVE ( 'NONE', #2993, #13096, #18112, .T. ) ;
#913 = CARTESIAN_POINT ( 'NONE',  ( -16.48417771855191205, 10.21602491043049810, 1.967329235809863297 ) ) ;
#914 = AXIS2_PLACEMENT_3D ( 'NONE', #18012, #10626, #23575 ) ;
#915 = DIRECTION ( 'NONE',  ( 0.000000000000000000, 1.000000000000000000, 0.000000000000000000 ) ) ;
#916 = CARTESIAN_POINT ( 'NONE',  ( -0.07248595781348986244, 27.43395343009157727, -2.169876273640742870 ) ) ;
#917 = ORIENTED_EDGE ( 'NONE', *, *, #4812, .T. ) ;
#918 = ORIENTED_EDGE ( 'NONE', *, *, #14010, .F. ) ;
#919 = DIRECTION ( 'NONE',  ( 0.000000000000000000, -1.000000000000000000, 0.000000000000000000 ) ) ;
#920 = CARTESIAN_POINT ( 'NONE',  ( 14.98162674931000105, 7.974294229383000143, 7.126218918095000632 ) ) ;
#921 = AXIS2_PLACEMENT_3D ( 'NONE', #17629, #21135, #23186 ) ;
#922 = CARTESIAN_POINT ( 'NONE',  ( -20.84720430363000077, -3.223876527765000333, -10.66212759214000094 ) ) ;
#923 = ADVANCED_FACE ( 'NONE', ( #1624 ), #23661, .F. ) ;
#924 = CARTESIAN_POINT ( 'NONE',  ( -15.28898322480000083, 9.440789260380000769, 4.024077471293999508 ) ) ;
#925 = CARTESIAN_POINT ( 'NONE',  ( -2.000000000000000000, 24.50000000000000000, 3.464101615137999968 ) ) ;
#926 = CARTESIAN_POINT ( 'NONE',  ( 14.85499951745999958, -9.268832152391000889, -2.910280560324999932 ) ) ;
#927 = CARTESIAN_POINT ( 'NONE',  ( -14.25243324638999809, -13.93375672974000068, -0.8660254037843999608 ) ) ;
#928 = PLANE ( 'NONE',  #23180 ) ;
#929 = B_SPLINE_CURVE_WITH_KNOTS ( 'NONE', 3,
 ( #8824, #12092, #6629, #14018, #3250 ),
 .UNSPECIFIED., .F., .F.,
 ( 4, 1, 4 ),
 ( 0.000000000000000000, 0.5000000000000000000, 1.000000000000000000 ),
 .UNSPECIFIED. ) ;
#930 = CARTESIAN_POINT ( 'NONE',  ( 24.42844379342591665, 9.716713767727441109, 2.075955529744581085 ) ) ;
#931 = ORIENTED_EDGE ( 'NONE', *, *, #5430, .T. ) ;
#932 = VECTOR ( 'NONE', #12319, 1000.000000000000000 ) ;
#933 = CARTESIAN_POINT ( 'NONE',  ( -0.1581195908683433182, 13.69161915620259151, 6.124206696172819875 ) ) ;
#934 = CARTESIAN_POINT ( 'NONE',  ( -0.2814148094397999622, 27.07250240009999942, -2.857252503208999705 ) ) ;
#935 = CARTESIAN_POINT ( 'NONE',  ( 1.596228967263000786, 11.66853105775998678, 4.467123007223999132 ) ) ;
#936 = EDGE_CURVE ( 'NONE', #12389, #16342, #3624, .T. ) ;
#937 = CARTESIAN_POINT ( 'NONE',  ( -20.11353743917332082, -9.187434725425410065, -1.202759340935936061 ) ) ;
#938 = CARTESIAN_POINT ( 'NONE',  ( -2.137330684254000079, 28.67937716036000140, 1.196956196243999848 ) ) ;
#939 = DIRECTION ( 'NONE',  ( -0.9999999999999994449, 3.360583440989998554E-08, -4.120678714624997717E-09 ) ) ;
#940 = CIRCLE ( 'NONE', #18358, 7.000000000000000000 ) ;
#941 = ORIENTED_EDGE ( 'NONE', *, *, #17551, .T. ) ;
#942 = DIRECTION ( 'NONE',  ( 0.000000000000000000, 1.000000000000000000, 0.000000000000000000 ) ) ;
#943 = ADVANCED_FACE ( 'NONE', ( #21849, #1742 ), #10714, .F. ) ;
#944 = CARTESIAN_POINT ( 'NONE',  ( 2.921430590333649935, 11.94558362360630177, 3.795594775063057202 ) ) ;
#945 = CARTESIAN_POINT ( 'NONE',  ( 4.106019081683001559, 14.61196862056002388, 4.606493351513002210 ) ) ;
#946 = EDGE_CURVE ( 'NONE', #4163, #21630, #17247, .T. ) ;
#947 = CARTESIAN_POINT ( 'NONE',  ( 0.2465075831868113188, 6.782055991726995359, 1.733133522506556057 ) ) ;
#948 = CARTESIAN_POINT ( 'NONE',  ( 0.000000000000000000, 15.09999999999999964, 0.000000000000000000 ) ) ;
#949 = CARTESIAN_POINT ( 'NONE',  ( -9.310023045028000155, 13.82947516575999991, -6.440908831219999797 ) ) ;
#950 = DIRECTION ( 'NONE',  ( 1.000000000000000000, 0.000000000000000000, 0.000000000000000000 ) ) ;
#951 = CARTESIAN_POINT ( 'NONE',  ( 14.79262625730999936, -7.984278194804999451, 4.494107504349000415 ) ) ;
#952 = CARTESIAN_POINT ( 'NONE',  ( 0.6543697108982093891, 27.43333333333333357, 2.434931691670787046 ) ) ;
#953 = VERTEX_POINT ( 'NONE', #23892 ) ;
#954 = EDGE_CURVE ( 'NONE', #9155, #6884, #15198, .T. ) ;
#955 = CARTESIAN_POINT ( 'NONE',  ( -22.26703117493464745, -4.632470568168542968, 8.021466634618056091 ) ) ;
#956 = CARTESIAN_POINT ( 'NONE',  ( 0.9155719665318000633, 29.41635474111000192, -2.565350663984000246 ) ) ;
#957 = CARTESIAN_POINT ( 'NONE',  ( -12.25000000000000000, 6.613190111079999767, -13.46349570337000046 ) ) ;
#958 = CARTESIAN_POINT ( 'NONE',  ( 0.9835805066508525041, 13.73841607712214241, -6.045557612536501146 ) ) ;
#959 = VERTEX_POINT ( 'NONE', #12646 ) ;
#960 = CARTESIAN_POINT ( 'NONE',  ( 0.000000000000000000, -1.550000000000000044, 0.000000000000000000 ) ) ;
#961 = CYLINDRICAL_SURFACE ( 'NONE', #4239, 3.000000000000000000 ) ;
#962 = FACE_OUTER_BOUND ( 'NONE', #5721, .T. ) ;
#963 = DIRECTION ( 'NONE',  ( 0.000000000000000000, 1.000000000000000000, 0.000000000000000000 ) ) ;
#964 = CARTESIAN_POINT ( 'NONE',  ( 15.81388418947362062, -8.259696827618725479, -6.316793570899937649 ) ) ;
#965 = CARTESIAN_POINT ( 'NONE',  ( -4.322696709239871815, 13.59640335390094634, 4.972036931828690776 ) ) ;
#966 = LINE ( 'NONE', #2675, #23567 ) ;
#967 = FACE_OUTER_BOUND ( 'NONE', #16594, .T. ) ;
#968 = EDGE_LOOP ( 'NONE', ( #9129, #8222, #23654, #14263 ) ) ;
#969 = FACE_OUTER_BOUND ( 'NONE', #3292, .T. ) ;
#970 = CARTESIAN_POINT ( 'NONE',  ( -2.922221168653406309, 11.94577451725421646, -3.794953772402525516 ) ) ;
#971 = ORIENTED_EDGE ( 'NONE', *, *, #12390, .T. ) ;
#972 = CARTESIAN_POINT ( 'NONE',  ( -23.50032910583999879, 1.512442827330999945E-14, 0.000000000000000000 ) ) ;
#973 = EDGE_CURVE ( 'NONE', #3560, #2047, #14455, .T. ) ;
#974 = CARTESIAN_POINT ( 'NONE',  ( -1.502369499347320447, 23.90757363759589893, 1.597718646107638474 ) ) ;
#975 = DIRECTION ( 'NONE',  ( 1.000000000000000000, 0.000000000000000000, 0.000000000000000000 ) ) ;
#976 = AXIS2_PLACEMENT_3D ( 'NONE', #11607, #4453, #18978 ) ;
#977 = CARTESIAN_POINT ( 'NONE',  ( 15.85478027152999836, -10.51359821371000081, 3.409925352663000009 ) ) ;
#978 = CARTESIAN_POINT ( 'NONE',  ( 4.000000000000000000, 26.50000000000000355, 0.000000000000000000 ) ) ;
#979 = CARTESIAN_POINT ( 'NONE',  ( 0.05636985319968999819, 26.77669433610000382, 2.870524099806999629 ) ) ;
#980 = B_SPLINE_CURVE_WITH_KNOTS ( 'NONE', 3,
 ( #19590, #14009, #21765, #10745, #21650, #23577, #23323, #10513, #17896, #6622 ),
 .UNSPECIFIED., .F., .F.,
 ( 4, 2, 2, 2, 4 ),
 ( 0.2499810176238006776, 0.4374857632178505984, 0.6249905088119004359, 0.8124952544059501625, 1.000000000000000000 ),
 .UNSPECIFIED. ) ;
#981 = ORIENTED_EDGE ( 'NONE', *, *, #7459, .F. ) ;
#982 = ADVANCED_BREP_SHAPE_REPRESENTATION ( '', ( #8659, #4390 ), #23331 ) ;
#983 = PLANE ( 'NONE',  #23592 ) ;
#984 = DIRECTION ( 'NONE',  ( 0.000000000000000000, 1.000000000000000000, 0.000000000000000000 ) ) ;
#985 = CARTESIAN_POINT ( 'NONE',  ( -20.15132910583999859, -9.188404534074999574, 1.125025998286999896E-14 ) ) ;
#986 = ORIENTED_EDGE ( 'NONE', *, *, #7332, .T. ) ;
#987 = EDGE_CURVE ( 'NONE', #13362, #22144, #4263, .T. ) ;
#988 = CARTESIAN_POINT ( 'NONE',  ( -23.00369019983000030, -5.232895320036999642, 9.395593148101001546 ) ) ;
#989 = CARTESIAN_POINT ( 'NONE',  ( 3.649794085728314208, 28.20197603011189713, -2.511592555635394852 ) ) ;
#990 = CARTESIAN_POINT ( 'NONE',  ( -1.672509921847626257, 28.00639765414753413, -3.652834497694421589 ) ) ;
#991 = CARTESIAN_POINT ( 'NONE',  ( 14.97294087919659056, 10.13249089077432785, 2.022385466357334405 ) ) ;
#992 = CARTESIAN_POINT ( 'NONE',  ( -16.75277932490000055, 10.95855636149000034, -1.542517388603999784 ) ) ;
#993 = VECTOR ( 'NONE', #6073, 1000.000000000000000 ) ;
#994 = CARTESIAN_POINT ( 'NONE',  ( 4.834780805419000238, 12.45065217972999960, 0.000000000000000000 ) ) ;
#995 = DIRECTION ( 'NONE',  ( 0.000000000000000000, -0.9998172265789604385, -0.01911840568550923769 ) ) ;
#996 = CARTESIAN_POINT ( 'NONE',  ( -4.630573125257002154, 12.42127774015998298, -1.209421156049999224 ) ) ;
#997 = AXIS2_PLACEMENT_3D ( 'NONE', #14640, #5794, #3629 ) ;
#998 = CARTESIAN_POINT ( 'NONE',  ( 0.000000000000000000, 23.00000000000000000, 0.000000000000000000 ) ) ;
#999 = CARTESIAN_POINT ( 'NONE',  ( -2.174360314446455611, 29.40514713709596961, 0.02075030649910500347 ) ) ;
#1000 = EDGE_LOOP ( 'NONE', ( #8543, #22260, #1976, #4442, #2164 ) ) ;
#1001 = CARTESIAN_POINT ( 'NONE',  ( -0.1522890450232986803, 24.04166422735650954, -2.528496764073642211 ) ) ;
#1002 = CARTESIAN_POINT ( 'NONE',  ( -15.62058162434104425, -7.748628952019913640, -6.926152932935100814 ) ) ;
#1003 = EDGE_LOOP ( 'NONE', ( #15205, #18643, #14623, #7226 ) ) ;
#1004 = CARTESIAN_POINT ( 'NONE',  ( 5.435972110109003275, 14.69581070629001474, -2.844462854985000178 ) ) ;
#1005 = CARTESIAN_POINT ( 'NONE',  ( -4.544340308300998998, 13.49051417780999884, -5.132142894851999593 ) ) ;
#1006 = CARTESIAN_POINT ( 'NONE',  ( -24.49999999999999289, 1.631301440766486310, -10.29771265513020850 ) ) ;
#1007 = CARTESIAN_POINT ( 'NONE',  ( 15.47718892131000068, -5.177634673800000975, -8.189908713891000502 ) ) ;
#1008 = ORIENTED_EDGE ( 'NONE', *, *, #13699, .F. ) ;
#1009 = CIRCLE ( 'NONE', #16482, 5.000000000000000000 ) ;
#1010 = CARTESIAN_POINT ( 'NONE',  ( -6.250000000000000000, 16.31160201366999729, -1.000000000001000089 ) ) ;
#1011 = CIRCLE ( 'NONE', #16100, 7.000000000000000000 ) ;
#1012 = CARTESIAN_POINT ( 'NONE',  ( 1.999167105995449889, 26.88333333333333641, -1.536366799937288086 ) ) ;
#1013 = CARTESIAN_POINT ( 'NONE',  ( 23.41677564524290744, 34.01856778792605240, 6.000000000000000000 ) ) ;
#1014 = VERTEX_POINT ( 'NONE', #20737 ) ;
#1015 = DIRECTION ( 'NONE',  ( 0.000000000000000000, 0.000000000000000000, -1.000000000000000000 ) ) ;
#1016 = CARTESIAN_POINT ( 'NONE',  ( -4.900699999999999612, 1.284663064832999817E-14, 0.000000000000000000 ) ) ;
#1017 = CARTESIAN_POINT ( 'NONE',  ( -23.44629291275694172, 5.369329345814918497, -7.615845659716430127 ) ) ;
#1018 = CARTESIAN_POINT ( 'NONE',  ( -14.00000000000000533, 0.8719941289985287947, 9.658611517165889282 ) ) ;
#1019 = CARTESIAN_POINT ( 'NONE',  ( 17.16962222460619358, 0.4914365713909190081, 10.41567669192089873 ) ) ;
#1020 = DIRECTION ( 'NONE',  ( 0.7071067750626029991, 0.7071067873022029993, -3.423807777995014990E-06 ) ) ;
#1021 = CARTESIAN_POINT ( 'NONE',  ( -14.42499036736162310, -9.146326703434620953, 9.158041868012015030 ) ) ;
#1022 = CARTESIAN_POINT ( 'NONE',  ( 20.96866900885000007, -10.17611281151999947, 4.721347032623000040 ) ) ;
#1023 = AXIS2_PLACEMENT_3D ( 'NONE', #10492, #4549, #1278 ) ;
#1024 = CARTESIAN_POINT ( 'NONE',  ( 0.000000000000000000, 15.04999987253367877, 0.000000000000000000 ) ) ;
#1025 = CARTESIAN_POINT ( 'NONE',  ( -3.899678468944780096, 13.96058569223144374, -4.846132543982858643 ) ) ;
#1026 = DIRECTION ( 'NONE',  ( 0.000000000000000000, 0.000000000000000000, -1.000000000000000000 ) ) ;
#1027 = ADVANCED_FACE ( 'NONE', ( #11423 ), #13339, .T. ) ;
#1028 = CARTESIAN_POINT ( 'NONE',  ( -1.997348637187154052, 30.15409434752375972, -0.8235051463819260675 ) ) ;
#1029 = EDGE_LOOP ( 'NONE', ( #20191, #6223, #8135, #10918 ) ) ;
#1030 = CARTESIAN_POINT ( 'NONE',  ( 23.56485220644000123, 10.89047681322000116, -1.152164691522000073 ) ) ;
#1031 = B_SPLINE_CURVE_WITH_KNOTS ( 'NONE', 3,
 ( #20391, #7536, #11544, #11309, #13341, #16986, #5956, #15272, #13463, #388, #20621, #11190, #6072, #7417, #503, #2208, #18573, #18924, #22435, #4031, #9599, #145, #16734, #7785, #4276, #19036, #13114, #15039, #34, #2333, #7665, #9722 ),
 .UNSPECIFIED., .F., .F.,
 ( 4, 2, 2, 2, 2, 2, 2, 2, 2, 2, 2, 2, 2, 2, 2, 4 ),
 ( 0.000000000000000000, 0.1250000000000003053, 0.1875000000000003331, 0.2187500000000004718, 0.2500000000000006106, 0.3125000000000006106, 0.3437500000000005551, 0.3750000000000004996, 0.5000000000000004441, 0.5625000000000004441, 0.5937500000000005551, 0.6250000000000006661, 0.6875000000000006661, 0.7187500000000006661, 0.7500000000000005551, 1.000000000000000000 ),
 .UNSPECIFIED. ) ;
#1032 = CARTESIAN_POINT ( 'NONE',  ( 24.18640269352763639, 8.182940205309693127, 6.768123944646319501 ) ) ;
#1033 = AXIS2_PLACEMENT_3D ( 'NONE', #4893, #17856, #19791 ) ;
#1034 = CARTESIAN_POINT ( 'NONE',  ( -1.536366799937282313, 27.55086340285666680, 1.999167105995454552 ) ) ;
#1035 = CARTESIAN_POINT ( 'NONE',  ( -1.523618227440715955, 24.32489914943822029, -1.660063800766738984 ) ) ;
#1036 = CARTESIAN_POINT ( 'NONE',  ( -11.04281598264000053, 1.359882291614000008E-14, 0.000000000000000000 ) ) ;
#1037 = CARTESIAN_POINT ( 'NONE',  ( -4.884003751836998752, 12.49132197575000092, -0.8076278545717995305 ) ) ;
#1038 = ORIENTED_EDGE ( 'NONE', *, *, #627, .T. ) ;
#1039 = CARTESIAN_POINT ( 'NONE',  ( -16.62373390469630863, 9.968533772034067653, -3.001379283816392185 ) ) ;
#1040 = CARTESIAN_POINT ( 'NONE',  ( -3.999709959627196110, 24.53198827073818578, -0.7544996412928929308 ) ) ;
#1041 = VECTOR ( 'NONE', #1026, 1000.000000000000000 ) ;
#1042 = CARTESIAN_POINT ( 'NONE',  ( 60.61494135913342518, 27.01856778792605240, -2.673746900119611247 ) ) ;
#1043 = CIRCLE ( 'NONE', #4136, 12.50000000000000000 ) ;
#1044 = DIRECTION ( 'NONE',  ( 0.000000000000000000, 1.000000000000000000, 0.000000000000000000 ) ) ;
#1045 = VERTEX_POINT ( 'NONE', #20976 ) ;
#1046 = CARTESIAN_POINT ( 'NONE',  ( 3.999999999999999112, 29.91068681084913905, -1.228746328088897721 ) ) ;
#1047 = AXIS2_PLACEMENT_3D ( 'NONE', #19546, #12406, #6941 ) ;
#1048 = CARTESIAN_POINT ( 'NONE',  ( -12.07716019469000024, 9.613013645102999050, -12.04164784824000023 ) ) ;
#1049 = FACE_OUTER_BOUND ( 'NONE', #9713, .T. ) ;
#1050 = CARTESIAN_POINT ( 'NONE',  ( -18.06675765898000208, -8.132406931018000051, 7.220925319278000742 ) ) ;
#1051 = CARTESIAN_POINT ( 'NONE',  ( 22.15395833333332121, -7.388848214911551082, -5.678196526935670896 ) ) ;
#1052 = CARTESIAN_POINT ( 'NONE',  ( 16.07374951746000136, 1.809993214902999803, 9.579455531516000377 ) ) ;
#1053 = CARTESIAN_POINT ( 'NONE',  ( 1.246850352501936765, 28.32748383450717711, -1.804444192914298695 ) ) ;
#1054 = CARTESIAN_POINT ( 'NONE',  ( 0.000000000000000000, 22.00000000000000000, 0.000000000000000000 ) ) ;
#1055 = EDGE_CURVE ( 'NONE', #6663, #12473, #16944, .T. ) ;
#1056 = CARTESIAN_POINT ( 'NONE',  ( 1.699986747157999911, 9.000014340785000400, 0.8485215224771999187 ) ) ;
#1057 = ORIENTED_EDGE ( 'NONE', *, *, #17739, .F. ) ;
#1058 = CARTESIAN_POINT ( 'NONE',  ( 1.934504865404305329, 13.87243343662209583, 5.816204379626650933 ) ) ;
#1059 = CARTESIAN_POINT ( 'NONE',  ( 2.361836001938000251, 25.88663313894999973, -0.7160459369172998967 ) ) ;
#1060 = AXIS2_PLACEMENT_3D ( 'NONE', #2053, #22506, #20579 ) ;
#1061 = DIRECTION ( 'NONE',  ( 1.000000000000000000, 0.000000000000000000, -1.253337711393242021E-14 ) ) ;
#1062 = CARTESIAN_POINT ( 'NONE',  ( -19.93064731917000287, 1.667734798046999867, 10.92226482541000010 ) ) ;
#1063 = VECTOR ( 'NONE', #16789, 1000.000000000000000 ) ;
#1064 = DIRECTION ( 'NONE',  ( 0.000000000000000000, 0.000000000000000000, -1.000000000000000000 ) ) ;
#1065 = ORIENTED_EDGE ( 'NONE', *, *, #23915, .F. ) ;
#1066 = APPLICATION_CONTEXT ( 'automotive_design' ) ;
#1067 = CARTESIAN_POINT ( 'NONE',  ( 4.649999999999999467, 20.00000000000000000, 0.000000000000000000 ) ) ;
#1068 = CARTESIAN_POINT ( 'NONE',  ( 4.675391681975701097, 12.38404500047236567, -1.288137502435812820 ) ) ;
#1069 = EDGE_CURVE ( 'NONE', #629, #17203, #20259, .T. ) ;
#1070 = CARTESIAN_POINT ( 'NONE',  ( -0.4616800974773001554, 13.20162905315999957, 6.080923912729003789 ) ) ;
#1071 = CARTESIAN_POINT ( 'NONE',  ( -8.000000000000000000, 10.50000000000000000, 0.000000000000000000 ) ) ;
#1072 = DIRECTION ( 'NONE',  ( 0.000000000000000000, -1.000000000000000000, 0.000000000000000000 ) ) ;
#1073 = CARTESIAN_POINT ( 'NONE',  ( -1.999167105995453442, 27.35086340285666395, -1.536366799937283645 ) ) ;
#1074 = CARTESIAN_POINT ( 'NONE',  ( -14.25521440656999950, -2.679375877985999743, 10.98274110836000084 ) ) ;
#1075 = VECTOR ( 'NONE', #23438, 1000.000000000000000 ) ;
#1076 = CARTESIAN_POINT ( 'NONE',  ( 18.54843892131000160, -5.767951301206999837, 7.596080989717999721 ) ) ;
#1077 = ADVANCED_FACE ( 'NONE', ( #19151, #385 ), #18683, .F. ) ;
#1078 = CARTESIAN_POINT ( 'NONE',  ( 18.92821040849097614, 2.505321190189683911, 10.13026339292191302 ) ) ;
#1079 = ORIENTED_EDGE ( 'NONE', *, *, #8643, .T. ) ;
#1080 = B_SPLINE_CURVE_WITH_KNOTS ( 'NONE', 3,
 ( #21557, #2531, #23107, #15843, #13667, #6769, #6283, #21188, #6405, #14162, #19376, #13786 ),
 .UNSPECIFIED., .F., .F.,
 ( 4, 1, 1, 1, 1, 2, 2, 4 ),
 ( 0.000000000000000000, 0.2499999999999980016, 0.3749999999999969469, 0.4374999999999963918, 0.4687499999999962252, 0.4843749999999963363, 0.4999999999999964473, 1.000000000000000000 ),
 .UNSPECIFIED. ) ;
#1081 = CARTESIAN_POINT ( 'NONE',  ( -0.6543697108982037269, 28.63333333333333641, -2.434931691670788823 ) ) ;
#1082 = CARTESIAN_POINT ( 'NONE',  ( -1.273196900314999880, 30.92615821231000339, -1.841387178119999968 ) ) ;
#1083 = PLANE ( 'NONE',  #21533 ) ;
#1084 = CARTESIAN_POINT ( 'NONE',  ( -2.511040024960635719, 13.99897430365290596, -5.586622607424842180 ) ) ;
#1085 = ORIENTED_EDGE ( 'NONE', *, *, #23142, .F. ) ;
#1087 = VECTOR ( 'NONE', #8395, 1000.000000000000000 ) ;
#1086 = PLANE ( 'NONE',  #5614 ) ;
#1088 = DIRECTION ( 'NONE',  ( 1.000000000000000000, 0.000000000000000000, 0.000000000000000000 ) ) ;
#1089 = EDGE_CURVE ( 'NONE', #18064, #16087, #22309, .T. ) ;
#1090 = DIRECTION ( 'NONE',  ( 0.000000000000000000, 0.000000000000000000, 1.000000000000000000 ) ) ;
#1091 = CARTESIAN_POINT ( 'NONE',  ( -2.000000000000000000, 23.50000000000000000, 0.000000000000000000 ) ) ;
#1092 = CARTESIAN_POINT ( 'NONE',  ( 15.45148061670815842, -8.690430497184191694, 5.949322236961282151 ) ) ;
#1093 = DIRECTION ( 'NONE',  ( 1.000000000000000000, 0.000000000000000000, 0.000000000000000000 ) ) ;
#1094 = CARTESIAN_POINT ( 'NONE',  ( 0.000000000000000000, 22.00000000000000000, 0.000000000000000000 ) ) ;
#1095 = CARTESIAN_POINT ( 'NONE',  ( -23.99212502903982980, -8.254180775415035143, 10.70333952211954198 ) ) ;
#1096 = EDGE_LOOP ( 'NONE', ( #6511, #10471, #14338, #13387 ) ) ;
#1097 = DIRECTION ( 'NONE',  ( 0.000000000000000000, 0.000000000000000000, -1.000000000000000000 ) ) ;
#1098 = CARTESIAN_POINT ( 'NONE',  ( -4.143590529358013974, 12.32185200877851905, -2.404200284871922388 ) ) ;
#1099 = AXIS2_PLACEMENT_3D ( 'NONE', #23876, #22181, #20021 ) ;
#1100 = EDGE_LOOP ( 'NONE', ( #9009, #12037, #22729, #307, #8287, #5800, #13151, #4308, #8031, #1436 ) ) ;
#1101 = CARTESIAN_POINT ( 'NONE',  ( -2.389125669399000174, 25.50974983101999882, -0.8775158854510999307 ) ) ;
#1102 = CARTESIAN_POINT ( 'NONE',  ( 6.131904361748996557, 14.49481577323998494, -0.05944742189950995986 ) ) ;
#1103 = EDGE_CURVE ( 'NONE', #23793, #12304, #11219, .T. ) ;
#1104 = CARTESIAN_POINT ( 'NONE',  ( -2.937971692690656944, 13.09510414649091103, 6.070550775144435640 ) ) ;
#1105 = CARTESIAN_POINT ( 'NONE',  ( 6.228968653373813780, 13.74531475821428472, -1.369654784524615421 ) ) ;
#1106 = DIRECTION ( 'NONE',  ( 0.000000000000000000, 1.000000000000000000, 0.000000000000000000 ) ) ;
#1107 = VECTOR ( 'NONE', #14524, 1000.000000000000000 ) ;
#1108 = LINE ( 'NONE', #7040, #6688 ) ;
#1109 = VERTEX_POINT ( 'NONE', #4029 ) ;
#1110 = CYLINDRICAL_SURFACE ( 'NONE', #20496, 10.59999999999999964 ) ;
#1111 = VECTOR ( 'NONE', #3507, 1000.000000000000114 ) ;
#1112 = CARTESIAN_POINT ( 'NONE',  ( 0.000000000000000000, 29.69999999999999929, 0.000000000000000000 ) ) ;
#1113 = CARTESIAN_POINT ( 'NONE',  ( 6.125000000000000000, 22.00000000000000000, 0.000000000000000000 ) ) ;
#1114 = VERTEX_POINT ( 'NONE', #15150 ) ;
#1115 = CARTESIAN_POINT ( 'NONE',  ( -18.87548909685999732, -9.583084618030000001, 1.668392796240999898 ) ) ;
#1116 = DIRECTION ( 'NONE',  ( 0.000000000000000000, -0.5000000000000169864, 0.8660254037844288266 ) ) ;
#1117 = CARTESIAN_POINT ( 'NONE',  ( 0.000000000000000000, 19.00000000000000000, 0.000000000000000000 ) ) ;
#1118 = CARTESIAN_POINT ( 'NONE',  ( 15.23231850497268525, 4.710292849053081099, 9.203326907294682613 ) ) ;
#1119 = CIRCLE ( 'NONE', #15016, 4.750000000000000000 ) ;
#1120 = DIRECTION ( 'NONE',  ( 0.000000000000000000, -1.000000000000000000, 0.000000000000000000 ) ) ;
#1121 = EDGE_CURVE ( 'NONE', #3998, #20964, #9719, .T. ) ;
#1122 = CARTESIAN_POINT ( 'NONE',  ( 4.834782059083999606, 12.44497316928999808, -0.3759403457470999466 ) ) ;
#1123 = DIRECTION ( 'NONE',  ( 8.117316429522999705E-13, 1.000000000000000000, 5.625558360782999934E-11 ) ) ;
#1124 = ADVANCED_FACE ( 'NONE', ( #22660 ), #11660, .T. ) ;
#1125 = CARTESIAN_POINT ( 'NONE',  ( -4.736748033549996073, 12.61325905412998871, 0.1514502988820001228 ) ) ;
#1126 = ORIENTED_EDGE ( 'NONE', *, *, #3156, .T. ) ;
#1127 = CARTESIAN_POINT ( 'NONE',  ( 8.124934037954998800, -12.44999999999999929, 0.000000000000000000 ) ) ;
#1128 = CIRCLE ( 'NONE', #19706, 3.100000000000000089 ) ;
#1129 = CARTESIAN_POINT ( 'NONE',  ( -1.286443996900747511, 29.52275116942843880, 1.737178360938291144 ) ) ;
#1130 = ORIENTED_EDGE ( 'NONE', *, *, #7876, .F. ) ;
#1131 = CARTESIAN_POINT ( 'NONE',  ( 1.259047450927246903, 29.33333333333332860, -2.184465970885645536 ) ) ;
#1132 = CARTESIAN_POINT ( 'NONE',  ( -16.54663518748942153, 8.347930828672053494, 6.471747366174584570 ) ) ;
#1133 = AXIS2_PLACEMENT_3D ( 'NONE', #9306, #16563, #21795 ) ;
#1134 = B_SPLINE_CURVE_WITH_KNOTS ( 'NONE', 3,
 ( #4597, #6278, #11858, #13423, #13661, #13910, #19241, #2654, #459, #20823, #2525, #17549, #9796, #22982, #8112, #4720, #17179, #19371, #19494, #20943, #10047, #21307, #10283, #575, #17432, #7982, #17303, #703, #15595, #947, #8343, #15354, #826, #6525, #6160, #8226, #4348, #6398, #11739, #13781, #15837, #14506, #5086, #21785, #8590, #3151, #20094, #10532, #19741, #8839 ),
 .UNSPECIFIED., .F., .F.,
 ( 4, 2, 2, 2, 2, 2, 2, 2, 2, 2, 1, 2, 2, 2, 2, 1, 2, 2, 2, 2, 2, 2, 2, 2, 2, 4 ),
 ( 0.000000000000000000, 0.06250000000000036082, 0.09375000000000056899, 0.1250000000000007772, 0.1875000000000012490, 0.2187500000000014155, 0.2343750000000014155, 0.2500000000000014433, 0.3125000000000014433, 0.3437500000000014433, 0.3593750000000013878, 0.3671875000000013878, 0.3750000000000013878, 0.4375000000000011657, 0.4687500000000011102, 0.4843750000000009992, 0.4921875000000009992, 0.5000000000000009992, 0.5625000000000007772, 0.6250000000000005551, 0.6875000000000005551, 0.7500000000000004441, 0.8125000000000003331, 0.8437500000000003331, 0.8750000000000002220, 1.000000000000000000 ),
 .UNSPECIFIED. ) ;
#1135 = ORIENTED_EDGE ( 'NONE', *, *, #7163, .T. ) ;
#1136 = CARTESIAN_POINT ( 'NONE',  ( -3.657438266360000245, 28.00000000000000000, 3.657438266360000245 ) ) ;
#1137 = CARTESIAN_POINT ( 'NONE',  ( 6.223523631586996174, 13.71390417251999949, -0.8158110508759003343 ) ) ;
#1138 = EDGE_CURVE ( 'NONE', #20052, #18819, #14065, .T. ) ;
#1139 = CARTESIAN_POINT ( 'NONE',  ( 11.99999999999999822, -4.059331642145825647, -8.012115679970065685 ) ) ;
#1140 = EDGE_CURVE ( 'NONE', #22006, #14445, #17840, .T. ) ;
#1141 = VECTOR ( 'NONE', #11951, 1000.000000000000000 ) ;
#1142 = CARTESIAN_POINT ( 'NONE',  ( -20.03205420454666452, -1.202231731695348138, -9.185343705029872297 ) ) ;
#1143 = CARTESIAN_POINT ( 'NONE',  ( 15.83268908530999930, -1.865934471007999917, -10.03576702404999921 ) ) ;
#1144 = ORIENTED_EDGE ( 'NONE', *, *, #1797, .F. ) ;
#1145 = DIRECTION ( 'NONE',  ( 0.000000000000000000, 0.9981468999026679167, -0.06085035919937799298 ) ) ;
#1146 = DIRECTION ( 'NONE',  ( -1.000000000000000000, 0.000000000000000000, 0.000000000000000000 ) ) ;
#1147 = DIRECTION ( 'NONE',  ( 0.000000000000000000, -0.9997423213046380264, -0.02270002185933085032 ) ) ;
#1148 = VECTOR ( 'NONE', #13158, 1000.000000000000114 ) ;
#1149 = EDGE_LOOP ( 'NONE', ( #20634, #17980, #22228, #22921, #20107, #8861, #1065, #23136 ) ) ;
#1150 = CARTESIAN_POINT ( 'NONE',  ( 11.72559253311346339, 12.88358093003557592, 2.684900464144857501 ) ) ;
#1151 = DIRECTION ( 'NONE',  ( 0.000000000000000000, -1.000000000000000000, 0.000000000000000000 ) ) ;
#1152 = CARTESIAN_POINT ( 'NONE',  ( -14.00000000000000178, 7.084868190922404274, 5.933636879945280995 ) ) ;
#1154 = CARTESIAN_POINT ( 'NONE',  ( 16.65500885062994740, 10.07209838378439670, -2.687555505311734816 ) ) ;
#1153 = VECTOR ( 'NONE', #22123, 999.9999999999998863 ) ;
#1155 = AXIS2_PLACEMENT_3D ( 'NONE', #18085, #10820, #995 ) ;
#1156 = DIRECTION ( 'NONE',  ( 0.000000000000000000, -0.9704651937236938863, -0.2412411817472984998 ) ) ;
#1157 = CARTESIAN_POINT ( 'NONE',  ( -14.47125383376745589, -9.790219516174829550, 8.042794959434482749 ) ) ;
#1158 = CARTESIAN_POINT ( 'NONE',  ( -4.059709635163400776, 13.79591589661956164, -4.865803654251010357 ) ) ;
#1159 = DIRECTION ( 'NONE',  ( 0.000000000000000000, 1.000000000000000000, 0.000000000000000000 ) ) ;
#1160 = CARTESIAN_POINT ( 'NONE',  ( -1.172166007576319391, 30.07693318280233541, -1.814140047937379707 ) ) ;
#1161 = ORIENTED_EDGE ( 'NONE', *, *, #13164, .T. ) ;
#1162 = CARTESIAN_POINT ( 'NONE',  ( 21.19327927328000172, 3.892238382344999970, -9.590411839331999033 ) ) ;
#1163 = CARTESIAN_POINT ( 'NONE',  ( 24.04453577521502794, 10.40724578197013805, 2.113084592499416381 ) ) ;
#1164 = DIRECTION ( 'NONE',  ( 0.000000000000000000, -1.000000000000000000, 0.000000000000000000 ) ) ;
#1165 = ORIENTED_EDGE ( 'NONE', *, *, #10326, .T. ) ;
#1166 = CARTESIAN_POINT ( 'NONE',  ( -1.751083909111127657, 24.51702249263829003, 1.418072448255935925 ) ) ;
#1167 = CARTESIAN_POINT ( 'NONE',  ( -24.17970357211695287, -12.87935348060794460, -2.692294542481509012 ) ) ;
#1168 = CARTESIAN_POINT ( 'NONE',  ( -0.6105871316501998436, 11.54226242508000233, -4.935054442950004727 ) ) ;
#1169 = VERTEX_POINT ( 'NONE', #17954 ) ;
#1170 = CARTESIAN_POINT ( 'NONE',  ( -16.70746761638316968, 8.693072922700327609, -5.728755917543943532 ) ) ;
#1171 = CARTESIAN_POINT ( 'NONE',  ( 16.98637625730999900, -6.405805545913000110, -6.631092424295999876 ) ) ;
#1172 = VERTEX_POINT ( 'NONE', #15989 ) ;
#1173 = AXIS2_PLACEMENT_3D ( 'NONE', #9633, #9751, #11343 ) ;
#1174 = CARTESIAN_POINT ( 'NONE',  ( 1.304922239495370340, 27.34765878667958461, -1.734344529965001325 ) ) ;
#1175 = DIRECTION ( 'NONE',  ( 0.000000000000000000, 0.000000000000000000, 1.000000000000000000 ) ) ;
#1176 = ORIENTED_EDGE ( 'NONE', *, *, #2264, .F. ) ;
#1177 = DIRECTION ( 'NONE',  ( 0.000000000000000000, 1.000000000000000000, 0.000000000000000000 ) ) ;
#1178 = CARTESIAN_POINT ( 'NONE',  ( 12.45881424931000048, -1.641155845125999768, -10.50071198764000080 ) ) ;
#1179 = CARTESIAN_POINT ( 'NONE',  ( -23.89835131802999868, 11.12127188689000157, 1.495067083984999989 ) ) ;
#1180 = CARTESIAN_POINT ( 'NONE',  ( -16.23858452724999779, -8.437247725758000527, 6.781230591525000406 ) ) ;
#1181 = CARTESIAN_POINT ( 'NONE',  ( 22.26733333333332254, -4.654919140148669143, -8.076101565712940911 ) ) ;
#1182 = CARTESIAN_POINT ( 'NONE',  ( 15.80244494526000132, 1.908725879256999880, 10.10239154523000060 ) ) ;
#1183 = CARTESIAN_POINT ( 'NONE',  ( 0.1826013610580650148, 28.39373671405435218, -2.164540525022182749 ) ) ;
#1184 = CARTESIAN_POINT ( 'NONE',  ( 2.900806500513820829, 26.43562577624027199, -2.944020739578862234 ) ) ;
#1185 = CARTESIAN_POINT ( 'NONE',  ( 15.61599999999999966, 9.072019050554999353, 0.000000000000000000 ) ) ;
#1186 = VERTEX_POINT ( 'NONE', #10453 ) ;
#1187 = CARTESIAN_POINT ( 'NONE',  ( 23.72055893949304561, -3.444828185086491690, 8.695936745105788290 ) ) ;
#1188 = CARTESIAN_POINT ( 'NONE',  ( 2.820196252569187934, 14.07833607265465758, 5.437106381143619771 ) ) ;
#1189 = CARTESIAN_POINT ( 'NONE',  ( 0.6890999691677728300, 24.78398118435500308, 2.016836597077809046 ) ) ;
#1190 = CARTESIAN_POINT ( 'NONE',  ( 3.821520914465099228, 26.24995697614777868, 2.412446024836691461 ) ) ;
#1191 = CARTESIAN_POINT ( 'NONE',  ( -14.13652826923847883, 9.034860340956925029, -1.094524698571601506 ) ) ;
#1192 = CARTESIAN_POINT ( 'NONE',  ( -22.24936801119999785, 10.93443063335000076, 1.977547908896999829 ) ) ;
#1193 = CARTESIAN_POINT ( 'NONE',  ( -4.196763389404418731, 12.21402715469226763, 2.415977519593344169 ) ) ;
#1194 = ORIENTED_EDGE ( 'NONE', *, *, #14275, .F. ) ;
#1195 = FACE_OUTER_BOUND ( 'NONE', #23097, .T. ) ;
#1196 = CARTESIAN_POINT ( 'NONE',  ( 3.000000000000000000, 23.00000000000000000, 0.000000000000000000 ) ) ;
#1197 = CARTESIAN_POINT ( 'NONE',  ( 0.7693602595439000824, 13.21609357992999456, 6.056548692576001258 ) ) ;
#1198 = CARTESIAN_POINT ( 'NONE',  ( -21.27917920454665790, 8.977395928926879876, 2.412738463204236794 ) ) ;
#1199 = CARTESIAN_POINT ( 'NONE',  ( -10.04281598263999875, 20.50000000000000000, 1.000000000000000000 ) ) ;
#1200 = ADVANCED_FACE ( 'NONE', ( #15753 ), #8625, .F. ) ;
#1201 = DIRECTION ( 'NONE',  ( 0.000000000000000000, 0.000000000000000000, -1.000000000000000000 ) ) ;
#1202 = CARTESIAN_POINT ( 'NONE',  ( -16.69277858220999988, 10.68419017778999880, -3.897213304429000491 ) ) ;
#1203 = CARTESIAN_POINT ( 'NONE',  ( 16.13531392131000075, 9.604728693984000643, 1.402583754804999971 ) ) ;
#1204 = CARTESIAN_POINT ( 'NONE',  ( 1.259047450927256895, 27.46666666666666501, 2.184465970885639763 ) ) ;
#1205 = ORIENTED_EDGE ( 'NONE', *, *, #11724, .F. ) ;
#1206 = CARTESIAN_POINT ( 'NONE',  ( 5.262221487413253129, 13.84847638346749044, 4.167423381671452098 ) ) ;
#1207 = CARTESIAN_POINT ( 'NONE',  ( -1.961028468976000028, 29.64181871290999837, 1.602965254429000064 ) ) ;
#1208 = CARTESIAN_POINT ( 'NONE',  ( -15.57853743917333311, 9.071057687409222581, 1.187525622282655124 ) ) ;
#1209 = DIRECTION ( 'NONE',  ( 0.000000000000000000, -0.5795667693381943986, 0.8149247571885935848 ) ) ;
#1210 = B_SPLINE_CURVE_WITH_KNOTS ( 'NONE', 3,
 ( #17375, #17133, #21259, #893, #22578, #4671, #15660, #528, #6472, #19063, #13367, #13856, #20768, #22690, #20039, #14349, #10231, #1018, #1516, #8906, #19685, #21740, #21854, #23296, #1271, #3340, #12423, #5154, #8783, #1152, #23547, #5265, #10717, #18109, #8657, #6834, #23179 ),
 .UNSPECIFIED., .F., .F.,
 ( 4, 2, 1, 2, 2, 1, 1, 2, 2, 1, 2, 2, 1, 1, 1, 1, 2, 2, 1, 1, 1, 2, 2, 4 ),
 ( 0.000000000000000000, 0.1250000000000004996, 0.1875000000000006106, 0.2187500000000006106, 0.2500000000000006106, 0.3125000000000004996, 0.3437500000000004996, 0.3593750000000004996, 0.3750000000000004996, 0.4375000000000005551, 0.4687500000000006661, 0.5000000000000006661, 0.6250000000000009992, 0.6875000000000013323, 0.7187500000000014433, 0.7343750000000013323, 0.7421875000000014433, 0.7500000000000014433, 0.8125000000000011102, 0.8437500000000009992, 0.8593750000000008882, 0.8671875000000007772, 0.8750000000000006661, 1.000000000000000000 ),
 .UNSPECIFIED. ) ;
#1211 = ORIENTED_EDGE ( 'NONE', *, *, #20206, .F. ) ;
#1212 = FACE_OUTER_BOUND ( 'NONE', #2416, .T. ) ;
#1213 = CARTESIAN_POINT ( 'NONE',  ( 0.000000000000000000, 23.69744247139000137, 0.000000000000000000 ) ) ;
#1214 = ADVANCED_FACE ( 'NONE', ( #4636 ), #4506, .T. ) ;
#1215 = DIRECTION ( 'NONE',  ( 1.000000000000000000, 0.000000000000000000, 0.000000000000000000 ) ) ;
#1216 = CARTESIAN_POINT ( 'NONE',  ( 15.39572622089800014, -7.354054053997821860, 7.547009246631161794 ) ) ;
#1217 = CARTESIAN_POINT ( 'NONE',  ( -4.076854769385132471, 13.78041422864121479, 4.870052410342037064 ) ) ;
#1218 = CARTESIAN_POINT ( 'NONE',  ( -21.77637077250666309, -7.380920199195522002, -5.672421320939294631 ) ) ;
#1219 = CARTESIAN_POINT ( 'NONE',  ( 20.35970603379665889, -8.954414562724045012, 2.406562392635347436 ) ) ;
#1220 = VERTEX_POINT ( 'NONE', #6564 ) ;
#1221 = DIRECTION ( 'NONE',  ( 0.000000000000000000, -0.01045465616390956094, 0.9999453485888589732 ) ) ;
#1222 = CARTESIAN_POINT ( 'NONE',  ( 12.28022044534097645, -7.993836135614808214, 11.15426966573714473 ) ) ;
#1223 = B_SPLINE_CURVE_WITH_KNOTS ( 'NONE', 3,
 ( #5114, #12495, #12612, #5571 ),
 .UNSPECIFIED., .F., .F.,
 ( 4, 4 ),
 ( 0.000000000000000000, 1.000000000000000000 ),
 .UNSPECIFIED. ) ;
#1224 = VERTEX_POINT ( 'NONE', #21342 ) ;
#1225 = CARTESIAN_POINT ( 'NONE',  ( -0.2548307053832999935, 23.76799284288000180, -2.407861897382000294 ) ) ;
#1226 = CARTESIAN_POINT ( 'NONE',  ( 30.87226923053214378, 37.01856778792605240, -2.673746900119611247 ) ) ;
#1227 = CARTESIAN_POINT ( 'NONE',  ( -1.425181558570351115, 12.87128047289576216, 6.531978145723615903 ) ) ;
#1228 = CARTESIAN_POINT ( 'NONE',  ( 12.50000000000000000, 13.93375672974000068, 0.000000000000000000 ) ) ;
#1229 = CARTESIAN_POINT ( 'NONE',  ( 2.184465970885645092, 27.66666666666667140, -1.259047450927249123 ) ) ;
#1230 = ADVANCED_FACE ( 'NONE', ( #23382 ), #15983, .F. ) ;
#1231 = LINE ( 'NONE', #15984, #14039 ) ;
#1232 = ORIENTED_EDGE ( 'NONE', *, *, #22821, .T. ) ;
#1233 = FACE_OUTER_BOUND ( 'NONE', #14772, .T. ) ;
#1234 = CARTESIAN_POINT ( 'NONE',  ( -1.959116242179748779, 26.23461873539890021, 0.8476554397138756913 ) ) ;
#1235 = DIRECTION ( 'NONE',  ( 1.000000000000000000, 0.000000000000000000, 0.000000000000000000 ) ) ;
#1236 = VERTEX_POINT ( 'NONE', #12142 ) ;
#1237 = CARTESIAN_POINT ( 'NONE',  ( -23.76167883585000240, 10.79930063205999957, 3.320022971283000501 ) ) ;
#1238 = LINE ( 'NONE', #8629, #11857 ) ;
#1239 = CARTESIAN_POINT ( 'NONE',  ( 15.12422319296440065, 7.823096909157138512, 6.778400638252913168 ) ) ;
#1240 = DIRECTION ( 'NONE',  ( 0.000000000000000000, 0.000000000000000000, -1.000000000000000000 ) ) ;
#1241 = CARTESIAN_POINT ( 'NONE',  ( -2.163699527451000026, 30.08248585635000083, -0.1363395057005999944 ) ) ;
#1242 = ADVANCED_FACE ( 'NONE', ( #23141 ), #3276, .F. ) ;
#1243 = CARTESIAN_POINT ( 'NONE',  ( -7.500000000000000000, 18.50000000000000000, -5.000000000000000000 ) ) ;
#1244 = CARTESIAN_POINT ( 'NONE',  ( -4.775989160958999058, 12.47797649990998359, -0.3237615643668999010 ) ) ;
#1245 = ORIENTED_EDGE ( 'NONE', *, *, #4475, .T. ) ;
#1246 = DIRECTION ( 'NONE',  ( 0.000000000000000000, -1.000000000000000000, 0.000000000000000000 ) ) ;
#1247 = AXIS2_PLACEMENT_3D ( 'NONE', #16175, #1177, #15929 ) ;
#1248 = CARTESIAN_POINT ( 'NONE',  ( -1.638949455867213079, 29.31355001292886797, -1.406705521346627297 ) ) ;
#1249 = ORIENTED_EDGE ( 'NONE', *, *, #11485, .T. ) ;
#1250 = DIRECTION ( 'NONE',  ( 0.000000000000000000, 0.000000000000000000, 1.000000000000000000 ) ) ;
#1251 = CARTESIAN_POINT ( 'NONE',  ( -16.31512179670237472, 1.090436056802820852, 10.50050333464076147 ) ) ;
#1252 = EDGE_CURVE ( 'NONE', #18988, #11301, #21592, .T. ) ;
#1253 = ORIENTED_EDGE ( 'NONE', *, *, #13521, .F. ) ;
#1254 = CARTESIAN_POINT ( 'NONE',  ( -2.218105065315603142, 30.46568852542990768, 1.261346933442557772 ) ) ;
#1255 = CARTESIAN_POINT ( 'NONE',  ( 5.513483907770004855, 14.23393714730998560, -2.574004873080997680 ) ) ;
#1256 = CARTESIAN_POINT ( 'NONE',  ( 0.3502059142680099546, 28.20197603011301624, 4.416610674642952539 ) ) ;
#1257 = CARTESIAN_POINT ( 'NONE',  ( 16.82469336267999793, 6.712115241498000096, 8.814690082545999061 ) ) ;
#1258 = EDGE_CURVE ( 'NONE', #9228, #1109, #20726, .T. ) ;
#1259 = CARTESIAN_POINT ( 'NONE',  ( -1.603077936557000038, 27.47506359724000191, -1.876963106047000007 ) ) ;
#1260 = CARTESIAN_POINT ( 'NONE',  ( 15.50362658531000193, -9.889101471244000408, -2.495492728532000104 ) ) ;
#1261 = EDGE_CURVE ( 'NONE', #11307, #551, #2937, .T. ) ;
#1262 = ORIENTED_EDGE ( 'NONE', *, *, #16370, .T. ) ;
#1263 = CARTESIAN_POINT ( 'NONE',  ( -11.02918649291999920, -11.29156741745999959, 9.124755533559000042 ) ) ;
#1264 = DIRECTION ( 'NONE',  ( 1.000000000000000000, 0.000000000000000000, 0.000000000000000000 ) ) ;
#1265 = DIRECTION ( 'NONE',  ( 0.9996708941621519351, 0.02565352539210875166, 3.160978645759844973E-14 ) ) ;
#1266 = EDGE_LOOP ( 'NONE', ( #12701, #18089 ) ) ;
#1267 = CARTESIAN_POINT ( 'NONE',  ( -24.05821396189999817, -9.114349543487000105, 1.114048544447999944 ) ) ;
#1268 = CARTESIAN_POINT ( 'NONE',  ( 11.66614181939630512, 12.78577920083404429, 2.854240613876971366 ) ) ;
#1269 = CARTESIAN_POINT ( 'NONE',  ( 22.23518289557183181, 6.552653103078741381, 8.300818614678858509 ) ) ;
#1270 = VECTOR ( 'NONE', #13225, 1000.000000000000114 ) ;
#1271 = CARTESIAN_POINT ( 'NONE',  ( -14.00000000000000178, 5.717788174535797019, 7.417575028664895598 ) ) ;
#1272 = CARTESIAN_POINT ( 'NONE',  ( 16.31493751112632040, 1.365414610549234631, -10.28867410738198629 ) ) ;
#1273 = DIRECTION ( 'NONE',  ( -1.000000000000000000, 0.000000000000000000, 0.000000000000000000 ) ) ;
#1274 = DIRECTION ( 'NONE',  ( -0.000000000000000000, 1.000000000000000000, 0.000000000000000000 ) ) ;
#1275 = EDGE_CURVE ( 'NONE', #3898, #15294, #15523, .T. ) ;
#1276 = EDGE_CURVE ( 'NONE', #9702, #13003, #19100, .T. ) ;
#1277 = CARTESIAN_POINT ( 'NONE',  ( 0.6950034797113096019, 26.37418302490043587, 4.217541707417931995 ) ) ;
#1278 = DIRECTION ( 'NONE',  ( 1.000000000000000000, 0.000000000000000000, 0.000000000000000000 ) ) ;
#1279 = CARTESIAN_POINT ( 'NONE',  ( -1.606116587811105001, 30.11053178658430340, -1.444150352961293793 ) ) ;
#1280 = ORIENTED_EDGE ( 'NONE', *, *, #7489, .T. ) ;
#1281 = CARTESIAN_POINT ( 'NONE',  ( -0.2703868746345000074, 25.22914974194000237, -2.319981033806999715 ) ) ;
#1282 = CARTESIAN_POINT ( 'NONE',  ( 19.94564619923999871, 6.840494197459999981, -9.103015306854999267 ) ) ;
#1283 = CARTESIAN_POINT ( 'NONE',  ( 22.59749320841400433, 1.050738802132360705, 10.52673552388134581 ) ) ;
#1284 = CARTESIAN_POINT ( 'NONE',  ( -2.097612193317242024, 23.63127982162329133, -0.4251272349260063477 ) ) ;
#1285 = ORIENTED_EDGE ( 'NONE', *, *, #583, .F. ) ;
#1286 = CYLINDRICAL_SURFACE ( 'NONE', #2168, 10.59999999999999964 ) ;
#1287 = DIRECTION ( 'NONE',  ( 0.000000000000000000, 0.9999453485888588622, 0.01045465616390955921 ) ) ;
#1288 = AXIS2_PLACEMENT_3D ( 'NONE', #15227, #5683, #9443 ) ;
#1289 = CARTESIAN_POINT ( 'NONE',  ( 1.437939696344002316, 11.60874954011002025, -4.772587024640002618 ) ) ;
#1290 = ORIENTED_EDGE ( 'NONE', *, *, #154, .F. ) ;
#1291 = CARTESIAN_POINT ( 'NONE',  ( -16.65164514192520429, 9.627632571596107525, -3.955004559287954358 ) ) ;
#1292 = FACE_OUTER_BOUND ( 'NONE', #3662, .T. ) ;
#1293 = EDGE_LOOP ( 'NONE', ( #2027, #12212 ) ) ;
#1294 = DIRECTION ( 'NONE',  ( -1.000000000000000000, 0.000000000000000000, 0.000000000000000000 ) ) ;
#1295 = CARTESIAN_POINT ( 'NONE',  ( -14.25243324638999809, -6.216878364870000340, -12.50000000000000000 ) ) ;
#1296 = EDGE_LOOP ( 'NONE', ( #5419, #8368, #9608, #1038, #2352, #17879, #3376 ) ) ;
#1297 = CARTESIAN_POINT ( 'NONE',  ( -10.04561490871999929, 16.32684872328999859, -1.000000000000000000 ) ) ;
#1298 = CARTESIAN_POINT ( 'NONE',  ( 12.56850174931000019, 2.370728120151999629, -10.36336111974000040 ) ) ;
#1299 = CARTESIAN_POINT ( 'NONE',  ( -22.40107856874000092, 10.65649927505999806, -0.3310050493610999789 ) ) ;
#1300 = CARTESIAN_POINT ( 'NONE',  ( -14.20728104755000132, -10.73719763778000136, -0.8140697014076999638 ) ) ;
#1302 = ADVANCED_FACE ( 'NONE', ( #22900 ), #11770, .F. ) ;
#1301 = DIRECTION ( 'NONE',  ( 0.000000000000000000, 0.000000000000000000, -1.000000000000000000 ) ) ;
#1303 = ADVANCED_FACE ( 'NONE', ( #6315 ), #5575, .F. ) ;
#1304 = CARTESIAN_POINT ( 'NONE',  ( 19.32374951746000136, 9.811947351814998441, 0.7349391902708000135 ) ) ;
#1305 = CARTESIAN_POINT ( 'NONE',  ( -2.004270392011611612, 26.94942393816377191, -0.9183958586233323951 ) ) ;
#1306 = PRODUCT_DEFINITION_FORMATION_WITH_SPECIFIED_SOURCE ( 'ANY', '', #20806, .NOT_KNOWN. ) ;
#1307 = CARTESIAN_POINT ( 'NONE',  ( 3.304996520289660733, 26.37418302490023692, -2.710661522857508388 ) ) ;
#1308 = DIRECTION ( 'NONE',  ( 0.000000000000000000, 1.000000000000000000, 0.000000000000000000 ) ) ;
#1309 = ORIENTED_EDGE ( 'NONE', *, *, #8194, .T. ) ;
#1310 = CARTESIAN_POINT ( 'NONE',  ( -17.08430420454666887, -5.598425178770643384, 7.284634173358401021 ) ) ;
#1311 = DIRECTION ( 'NONE',  ( -1.000000000000000000, 0.000000000000000000, 0.000000000000000000 ) ) ;
#1313 = CIRCLE ( 'NONE', #11367, 0.9999999999999995559 ) ;
#1312 = CARTESIAN_POINT ( 'NONE',  ( 2.245636445399999737, 26.56119850838000218, -0.3106091461882000138 ) ) ;
#1314 = CARTESIAN_POINT ( 'NONE',  ( 3.560623727957782592, 26.31534065533139710, 2.563075085697512190 ) ) ;
#1315 = CARTESIAN_POINT ( 'NONE',  ( -19.48508853042000055, -10.46451423961999794, 1.868989650143999981 ) ) ;
#1316 = CARTESIAN_POINT ( 'NONE',  ( -2.142505351569140792, 11.67753982942237378, 4.317242088958800572 ) ) ;
#1317 = EDGE_LOOP ( 'NONE', ( #11536, #22718, #18025, #6085 ) ) ;
#1318 = FACE_OUTER_BOUND ( 'NONE', #12289, .T. ) ;
#1319 = CARTESIAN_POINT ( 'NONE',  ( -24.47970833437514671, -1.023963593989784870, -12.49997010189743563 ) ) ;
#1320 = CARTESIAN_POINT ( 'NONE',  ( 2.649379677055639259, 28.02555747447238943, 3.089210087447479491 ) ) ;
#1321 = CARTESIAN_POINT ( 'NONE',  ( -20.59892920454666410, -8.038787966541713459, 4.633122357395726532 ) ) ;
#1322 = CIRCLE ( 'NONE', #14832, 2.399999999999999911 ) ;
#1323 = ORIENTED_EDGE ( 'NONE', *, *, #10262, .T. ) ;
#1324 =( BOUNDED_SURFACE ( )  B_SPLINE_SURFACE ( 3, 3, ( 
 ( #17242, #9621, #7686, #4293, #6341, #17126 ),
 ( #20886, #15416, #17006, #19056, #405, #5865 ),
 ( #7925, #13251, #11682, #2469, #20642, #522 ),
 ( #15176, #4053, #7804, #9740, #9860, #15292 ) ),
 .UNSPECIFIED., .F., .F., .T. ) 
 B_SPLINE_SURFACE_WITH_KNOTS ( ( 4, 4 ),
 ( 4, 1, 1, 4 ),
 ( 0.000000000000000000, 1.000000000000000000 ),
 ( 0.9657854881572999206, 0.9726412705193000496, 0.9856983999281999642, 0.9888385341825000063 ),
 .UNSPECIFIED. ) 
 GEOMETRIC_REPRESENTATION_ITEM ( )  RATIONAL_B_SPLINE_SURFACE ( (
 ( 1.047483055770999982, 1.047483055770999982, 1.047483055770999982, 1.047483055770999982, 1.047483055770999982, 1.047483055770999982),
 ( 0.9841723147430000429, 0.9841723147430000429, 0.9841723147430000429, 0.9841723147430000429, 0.9841723147430000429, 0.9841723147430000429),
 ( 0.9841723147430000429, 0.9841723147430000429, 0.9841723147430000429, 0.9841723147430000429, 0.9841723147430000429, 0.9841723147430000429),
 ( 1.047483055770999982, 1.047483055770999982, 1.047483055770999982, 1.047483055770999982, 1.047483055770999982, 1.047483055770999982) ) ) 
 REPRESENTATION_ITEM ( '' )  SURFACE ( )  );
#1325 = DIRECTION ( 'NONE',  ( -1.000000000000000000, 0.000000000000000000, 0.000000000000000000 ) ) ;
#1326 = CARTESIAN_POINT ( 'NONE',  ( -15.06773579844999844, 6.079600582824999933, -9.557752359651999541 ) ) ;
#1327 = CARTESIAN_POINT ( 'NONE',  ( 15.58687642131000040, -1.771707419409999984, -9.528874100789000323 ) ) ;
#1328 = CARTESIAN_POINT ( 'NONE',  ( 18.45452326807764720, 9.933489636791392741, -3.151000111601911069 ) ) ;
#1329 = VERTEX_POINT ( 'NONE', #17591 ) ;
#1330 = CARTESIAN_POINT ( 'NONE',  ( 12.52688711657000020, -13.93375672974000068, -0.8660254037843999608 ) ) ;
#1331 = CARTESIAN_POINT ( 'NONE',  ( 2.487975651965000257, 29.17856066959000216, -0.4744621780437000003 ) ) ;
#1332 = AXIS2_PLACEMENT_3D ( 'NONE', #10810, #12736, #5236 ) ;
#1333 = B_SPLINE_CURVE_WITH_KNOTS ( 'NONE', 3,
 ( #18317, #11286, #20365, #18663, #23872, #3776, #11044, #7055, #9225, #18550, #14439, #5246, #14, #16715, #7398, #22176, #19259, #5932, #15127, #4006 ),
 .UNSPECIFIED., .F., .F.,
 ( 4, 2, 2, 1, 1, 2, 2, 2, 2, 2, 4 ),
 ( 0.000000000000000000, 0.2499999999999911737, 0.3749999999999851785, 0.4374999999999799050, 0.4687499999999784062, 0.4843749999999780176, 0.4999999999999776845, 0.6249999999999839018, 0.6874999999999863443, 0.7499999999999887867, 1.000000000000000000 ),
 .UNSPECIFIED. ) ;
#1334 = CARTESIAN_POINT ( 'NONE',  ( -14.89828743917333398, -7.239954394872571974, 5.563771113903599463 ) ) ;
#1335 = CARTESIAN_POINT ( 'NONE',  ( 3.128306947727627740, 14.16607981661443461, -5.265925022374893238 ) ) ;
#1336 = ORIENTED_EDGE ( 'NONE', *, *, #20077, .F. ) ;
#1337 = DIRECTION ( 'NONE',  ( 1.000000000000000000, 0.000000000000000000, 0.000000000000000000 ) ) ;
#1338 = CARTESIAN_POINT ( 'NONE',  ( -24.11803009775520934, -13.00903097537756992, 2.467105211282460964 ) ) ;
#1339 = CARTESIAN_POINT ( 'NONE',  ( 16.14508333333333212, -2.378018344083014490, 8.849171197995115534 ) ) ;
#1340 = FACE_OUTER_BOUND ( 'NONE', #2755, .T. ) ;
#1341 = LINE ( 'NONE', #10303, #13747 ) ;
#1342 = CARTESIAN_POINT ( 'NONE',  ( 0.8370874130355989706, 11.55651838240000195, 4.900516244706000890 ) ) ;
#1343 = EDGE_CURVE ( 'NONE', #19206, #4168, #8387, .T. ) ;
#1344 = CARTESIAN_POINT ( 'NONE',  ( -12.25000000000000355, 7.259277535838063677, -12.86049852923413539 ) ) ;
#1345 = ORIENTED_EDGE ( 'NONE', *, *, #20031, .F. ) ;
#1346 = DIRECTION ( 'NONE',  ( 0.000000000000000000, -1.000000000000000000, 0.000000000000000000 ) ) ;
#1347 = CARTESIAN_POINT ( 'NONE',  ( -4.000000000000000000, 26.24995697614769341, 2.103311180602513986 ) ) ;
#1348 = EDGE_LOOP ( 'NONE', ( #23222, #2521, #7520, #9139 ) ) ;
#1349 = CARTESIAN_POINT ( 'NONE',  ( -0.2740503536635999771, 23.87342747345000049, -2.589465832062999961 ) ) ;
#1350 = CARTESIAN_POINT ( 'NONE',  ( -19.10482910584000038, 1.458613477275000161E-14, 0.000000000000000000 ) ) ;
#1351 = CARTESIAN_POINT ( 'NONE',  ( 12.52688711657000020, 6.216878364870000340, -12.50000000000000000 ) ) ;
#1352 = FACE_OUTER_BOUND ( 'NONE', #11148, .T. ) ;
#1353 = CARTESIAN_POINT ( 'NONE',  ( 13.49999999999999645, -1.222753220167238863, 10.22419479022183708 ) ) ;
#1354 = DIRECTION ( 'NONE',  ( -0.7071067811866525998, 0.000000000000000000, -0.7071067811864425456 ) ) ;
#1355 = EDGE_LOOP ( 'NONE', ( #7560, #5400, #15054, #407 ) ) ;
#1356 = DIRECTION ( 'NONE',  ( 1.000000000000000000, 0.000000000000000000, 0.000000000000000000 ) ) ;
#1357 = AXIS2_PLACEMENT_3D ( 'NONE', #18081, #21470, #8753 ) ;
#1358 = LINE ( 'NONE', #21591, #9002 ) ;
#1359 = DIRECTION ( 'NONE',  ( 0.000000000000000000, 0.000000000000000000, 1.000000000000000000 ) ) ;
#1360 = VERTEX_POINT ( 'NONE', #23263 ) ;
#1361 = CARTESIAN_POINT ( 'NONE',  ( -21.38886788576999720, 8.715394838837001501, 5.275457124725000391 ) ) ;
#1362 = FACE_OUTER_BOUND ( 'NONE', #5374, .T. ) ;
#1363 = CARTESIAN_POINT ( 'NONE',  ( 15.23219685105820709, 4.714089901989198417, 9.201376909055083431 ) ) ;
#1364 = AXIS2_PLACEMENT_3D ( 'NONE', #11045, #22067, #15 ) ;
#1365 = CARTESIAN_POINT ( 'NONE',  ( 3.999709959623201971, 24.53198827073818933, 0.7544996413140969693 ) ) ;
#1366 = CARTESIAN_POINT ( 'NONE',  ( 2.322667919087999966, 30.40790453936999782, -0.4211969760945999952 ) ) ;
#1367 = CARTESIAN_POINT ( 'NONE',  ( 13.50000000000000000, 4.517872873748999929, -7.804362139085999850 ) ) ;
#1368 = CARTESIAN_POINT ( 'NONE',  ( 3.118557983420002344, 12.06593937194998922, -3.608953852771001447 ) ) ;
#1369 = ORIENTED_EDGE ( 'NONE', *, *, #23767, .T. ) ;
#1370 = CARTESIAN_POINT ( 'NONE',  ( -22.18617920454664727, -9.000065539970952599, -2.418830751902067533 ) ) ;
#1371 = EDGE_CURVE ( 'NONE', #11130, #22702, #21894, .T. ) ;
#1372 = ORIENTED_EDGE ( 'NONE', *, *, #11941, .F. ) ;
#1373 = CARTESIAN_POINT ( 'NONE',  ( -9.000000000000000000, 19.50000000000000000, -1.000000000000000000 ) ) ;
#1374 = DIRECTION ( 'NONE',  ( 0.000000000000000000, 1.000000000000000000, 0.000000000000000000 ) ) ;
#1375 = EDGE_LOOP ( 'NONE', ( #7092, #3096, #7354, #23291 ) ) ;
#1376 = CARTESIAN_POINT ( 'NONE',  ( 12.52688711657000020, -13.93375672974000068, -0.8660254037843999608 ) ) ;
#1377 = CARTESIAN_POINT ( 'NONE',  ( 12.00000000000000000, -6.717641695603743024, -5.958818398439713171 ) ) ;
#1378 = B_SPLINE_CURVE_WITH_KNOTS ( 'NONE', 3,
 ( #13207, #2184, #22177, #5589, #15128, #9696, #9462, #4255, #16837, #20598, #476, #22526, #5933, #11643 ),
 .UNSPECIFIED., .F., .F.,
 ( 4, 2, 2, 2, 2, 2, 4 ),
 ( 0.000000000000000000, 0.1249999999999985290, 0.1874999999999984734, 0.2499999999999984457, 0.3749999999999983347, 0.4999999999999983347, 1.000000000000000000 ),
 .UNSPECIFIED. ) ;
#1379 = CARTESIAN_POINT ( 'NONE',  ( 15.77581727657000066, -6.549303922337999850, -8.900682842320000177 ) ) ;
#1380 = CARTESIAN_POINT ( 'NONE',  ( 0.04846321314155000587, 26.98756359724000120, 2.467893978438000069 ) ) ;
#1381 = ADVANCED_FACE ( 'NONE', ( #5 ), #10686, .T. ) ;
#1382 = ORIENTED_EDGE ( 'NONE', *, *, #7490, .F. ) ;
#1383 = FACE_OUTER_BOUND ( 'NONE', #11764, .T. ) ;
#1384 = CARTESIAN_POINT ( 'NONE',  ( 13.50000000000000178, 9.568802105555617388, -0.1296229622023596650 ) ) ;
#1385 = SURFACE_STYLE_FILL_AREA ( #15784 ) ;
#1386 = VERTEX_POINT ( 'NONE', #11152 ) ;
#1387 = CARTESIAN_POINT ( 'NONE',  ( -23.03001354826000124, 9.280677558483001022, 2.853289170403999986 ) ) ;
#1388 = CARTESIAN_POINT ( 'NONE',  ( 11.36448692219687651, 9.446283672483898997, 8.638507912450332782 ) ) ;
#1389 = CARTESIAN_POINT ( 'NONE',  ( 23.47059551751145179, 4.797115948774011152, -9.456088267976967998 ) ) ;
#1390 = CIRCLE ( 'NONE', #5627, 12.44999999999999574 ) ;
#1391 = CARTESIAN_POINT ( 'NONE',  ( 0.000000000000000000, 20.00000000000000000, 0.000000000000000000 ) ) ;
#1392 = CARTESIAN_POINT ( 'NONE',  ( 16.27550863102649359, -0.04483518904284756329, -10.36594529132968923 ) ) ;
#1393 = EDGE_CURVE ( 'NONE', #22764, #1513, #151, .T. ) ;
#1394 = DIRECTION ( 'NONE',  ( -1.345659694784736864E-09, -1.000000000000000000, 0.000000000000000000 ) ) ;
#1395 = B_SPLINE_CURVE_WITH_KNOTS ( 'NONE', 3,
 ( #3563, #18223, #7534, #18333, #5490 ),
 .UNSPECIFIED., .F., .F.,
 ( 4, 1, 4 ),
 ( 0.000000000000000000, 0.5000000000000000000, 1.000000000000000000 ),
 .UNSPECIFIED. ) ;
#1396 = CARTESIAN_POINT ( 'NONE',  ( -1.018716668670999859, 30.37106448208000131, 1.936711703186000166 ) ) ;
#1397 = CARTESIAN_POINT ( 'NONE',  ( -15.59561067990999916, -1.941903525450000112, 10.08593956198000008 ) ) ;
#1398 = ADVANCED_FACE ( 'NONE', ( #18306 ), #5347, .F. ) ;
#1399 = CARTESIAN_POINT ( 'NONE',  ( 0.9774796333180513219, 29.94423007303124251, -1.927981652679361391 ) ) ;
#1400 = ORIENTED_EDGE ( 'NONE', *, *, #8012, .F. ) ;
#1401 = CARTESIAN_POINT ( 'NONE',  ( 11.09594815123491074, 11.32305097982894182, -5.387897831827406669 ) ) ;
#1402 = CARTESIAN_POINT ( 'NONE',  ( 23.61893502027211511, 3.101547904345725915, -10.14056206740493593 ) ) ;
#1403 = CARTESIAN_POINT ( 'NONE',  ( -1.182437155214619562, 23.61728437556105931, -1.756346252138746289 ) ) ;
#1404 = ORIENTED_EDGE ( 'NONE', *, *, #22713, .F. ) ;
#1405 = CARTESIAN_POINT ( 'NONE',  ( 11.01624327026000039, 12.44999999999999929, 0.000000000000000000 ) ) ;
#1406 = DIRECTION ( 'NONE',  ( 1.000000000000000000, 0.000000000000000000, 0.000000000000000000 ) ) ;
#1407 = CIRCLE ( 'NONE', #8349, 4.649999999999999467 ) ;
#1408 = CARTESIAN_POINT ( 'NONE',  ( 3.883475859697001376, 12.07688333241999068, -3.051465999718002475 ) ) ;
#1409 = ORIENTED_EDGE ( 'NONE', *, *, #14537, .T. ) ;
#1410 = EDGE_CURVE ( 'NONE', #7085, #18414, #4413, .T. ) ;
#1411 = CARTESIAN_POINT ( 'NONE',  ( 16.54762625731000014, -6.940875756134999186, 6.051234330564000174 ) ) ;
#1412 = VERTEX_POINT ( 'NONE', #3304 ) ;
#1413 = CARTESIAN_POINT ( 'NONE',  ( -2.037157279014845113, 26.87920215101449273, 0.8280411290571204619 ) ) ;
#1414 = CONTEXT_DEPENDENT_SHAPE_REPRESENTATION ( #19171, #4579 ) ;
#1415 = CARTESIAN_POINT ( 'NONE',  ( -23.75701756399666209, -13.93375672974000068, -0.3849425590144652243 ) ) ;
#1416 = ORIENTED_EDGE ( 'NONE', *, *, #2707, .T. ) ;
#1417 = DIRECTION ( 'NONE',  ( -1.000000000000000000, 0.000000000000000000, 0.000000000000000000 ) ) ;
#1418 = CARTESIAN_POINT ( 'NONE',  ( -4.032879115117613544, 14.96244278679635187, -4.610086244949046730 ) ) ;
#1419 = CARTESIAN_POINT ( 'NONE',  ( -22.18849929921000097, -0.6770054873877999757, 10.11404905110999941 ) ) ;
#1420 = CARTESIAN_POINT ( 'NONE',  ( -13.86707078901000045, 5.903954493066000175, -8.344675977248000365 ) ) ;
#1421 = CARTESIAN_POINT ( 'NONE',  ( -5.403725322399998809, 14.30357683451000739, -5.155213201826003733 ) ) ;
#1422 = CARTESIAN_POINT ( 'NONE',  ( -23.62400123529080176, 3.021837668578921221, 10.14788162303472596 ) ) ;
#1423 = CARTESIAN_POINT ( 'NONE',  ( -1.829580058295768197, 27.87696425337853157, 1.172525041583718952 ) ) ;
#1424 = CIRCLE ( 'NONE', #7199, 9.651424765286998664 ) ;
#1425 = CIRCLE ( 'NONE', #622, 12.50000000000000533 ) ;
#1426 = DIRECTION ( 'NONE',  ( -1.000000000000000000, 0.000000000000000000, 0.000000000000000000 ) ) ;
#1427 = ADVANCED_FACE ( 'NONE', ( #9215 ), #13691, .F. ) ;
#1428 = CARTESIAN_POINT ( 'NONE',  ( 0.8316999784727749923, 30.75381617240658727, -2.001085836244213656 ) ) ;
#1429 = VERTEX_POINT ( 'NONE', #14321 ) ;
#1430 = ADVANCED_FACE ( 'NONE', ( #12620, #20130 ), #16593, .F. ) ;
#1431 = CARTESIAN_POINT ( 'NONE',  ( -2.000000000000000000, 26.50000000000000355, -3.464101615137999968 ) ) ;
#1432 = CARTESIAN_POINT ( 'NONE',  ( 3.957520350577631074, 14.44398668127747953, 4.674802188335122288 ) ) ;
#1433 = CARTESIAN_POINT ( 'NONE',  ( -2.456483904114000083, 27.83663313894999902, -0.2419425476017999788 ) ) ;
#1434 = CARTESIAN_POINT ( 'NONE',  ( -1.271041439915000071, 26.35771896306000173, 1.902247796447000150 ) ) ;
#1435 = FACE_OUTER_BOUND ( 'NONE', #2398, .T. ) ;
#1436 = ORIENTED_EDGE ( 'NONE', *, *, #987, .T. ) ;
#1437 = DIRECTION ( 'NONE',  ( -1.000000000000000000, 0.000000000000000000, 0.000000000000000000 ) ) ;
#1438 = CARTESIAN_POINT ( 'NONE',  ( -24.41904027020278534, -2.048447027932289721, -12.49998758062248072 ) ) ;
#1439 = EDGE_CURVE ( 'NONE', #6590, #8278, #6877, .T. ) ;
#1440 = DIRECTION ( 'NONE',  ( 1.000000000000000000, 0.000000000000000000, 0.000000000000000000 ) ) ;
#1441 = EDGE_CURVE ( 'NONE', #9887, #10277, #1709, .T. ) ;
#1442 = AXIS2_PLACEMENT_3D ( 'NONE', #8505, #8620, #21815 ) ;
#1443 = CARTESIAN_POINT ( 'NONE',  ( -20.97684587121333166, 2.410473131623945608, 8.969936553441268501 ) ) ;
#1444 = ORIENTED_EDGE ( 'NONE', *, *, #5542, .T. ) ;
#1445 = CARTESIAN_POINT ( 'NONE',  ( -2.181170733482575841, 30.72643194342732897, -0.6746858939111454179 ) ) ;
#1446 = DIRECTION ( 'NONE',  ( 0.000000000000000000, 1.000000000000000000, 0.000000000000000000 ) ) ;
#1447 = CARTESIAN_POINT ( 'NONE',  ( 17.78062642131000004, 8.824178357484999680, -4.146495103786000058 ) ) ;
#1448 = CARTESIAN_POINT ( 'NONE',  ( 18.51438200485527474, 10.36799380519708613, -1.084925629257029511 ) ) ;
#1449 = ORIENTED_EDGE ( 'NONE', *, *, #13356, .F. ) ;
#1450 = CARTESIAN_POINT ( 'NONE',  ( 1.259047450927246903, 28.53333333333332789, -2.184465970885645536 ) ) ;
#1451 = CARTESIAN_POINT ( 'NONE',  ( 1.669522189709000015, 29.04620122864000109, 1.904710300619000263 ) ) ;
#1452 = DIRECTION ( 'NONE',  ( -1.000000000000000000, 0.000000000000000000, 0.000000000000000000 ) ) ;
#1453 = CARTESIAN_POINT ( 'NONE',  ( 0.000000000000000000, 21.89999999999999858, 0.000000000000000000 ) ) ;
#1454 = CIRCLE ( 'NONE', #4153, 2.000000000000000000 ) ;
#1455 = VERTEX_POINT ( 'NONE', #9099 ) ;
#1456 = CARTESIAN_POINT ( 'NONE',  ( 0.000000000000000000, 21.89999999999999858, 0.000000000000000000 ) ) ;
#1457 = DIRECTION ( 'NONE',  ( 1.000000000000000000, 0.000000000000000000, 0.000000000000000000 ) ) ;
#1458 = B_SPLINE_SURFACE_WITH_KNOTS ( 'NONE', 3, 3, ( 
 ( #5157, #3570, #16630, #14696, #7307, #5268, #10845, #3225, #5386, #23551, #19925, #3681, #12773, #14352, #40, #11072, #22089, #6961, #12654, #12426, #18455, #16510, #16150, #23781, #1520, #10607, #10721, #14231, #7188, #21626, #20045, #5498, #18339, #3461, #1865 ),
 ( #1748, #5044, #3343, #18229, #19810, #20162, #14577, #8908, #23899, #18115, #17991, #1396, #21744, #16275, #8787, #23668, #7078, #14464, #1631, #21972, #11314, #9726, #13120, #16863, #18578, #4280, #18805, #11549, #22316, #15045, #17109, #5733, #15159, #3802, #507 ),
 ( #20746, #7907, #1983, #2097, #14805, #9486, #11668, #9366, #13468, #12995, #2451, #22440, #5613, #9605, #5960, #15276, #22668, #20626, #5850, #16991, #16741, #265, #150, #7671, #392, #6077, #13233, #22554, #7542, #2213, #14922, #22200, #4036, #11431, #20396 ),
 ( #20871, #7790, #13345, #19041, #18929, #4152, #9843, #2338, #17223, #7423, #11196, #20517, #3922, #18690, #10088, #13588, #752, #11786, #23270, #9961, #21471, #6684, #17474, #12150, #19414, #21349, #12031, #21231, #23151, #15399, #10333, #22788, #868, #3074, #21103 ) ),
 .UNSPECIFIED., .F., .F., .F.,
 ( 4, 4 ),
 ( 4, 1, 1, 1, 1, 1, 1, 1, 1, 1, 1, 1, 1, 1, 1, 1, 1, 1, 1, 1, 1, 1, 1, 1, 1, 1, 1, 1, 1, 1, 1, 1, 4 ),
 ( -0.2678694646895999898, 1.311704223562000005 ),
 ( 0.2474280914112999830, 0.2714070983026000139, 0.2953861051939000171, 0.3193651120852000203, 0.3433441189764999679, 0.3673231258677999711, 0.3913021327591000298, 0.4152811396504000330, 0.4392601465417000361, 0.4632391534331000149, 0.4872181603244000181, 0.5111971672156999658, 0.5351761741069999134, 0.5591551809982999721, 0.5831341878895999198, 0.6071131947808999785, 0.6310922016721999261, 0.6550712085634999848, 0.6790502154547999325, 0.7030292223460999912, 0.7270082292373999389, 0.7509872361286999976, 0.7749662430200000562, 0.7989452499113000039, 0.8229242568026999827, 0.8469032636939999303, 0.8708822705852999890, 0.8948612774765999367, 0.9188402843678999954, 0.9428192912591999431, 0.9667982981504998907, 0.9907773050418000604, 1.014756311932999866 ),
 .UNSPECIFIED. ) ;
#1459 = CARTESIAN_POINT ( 'NONE',  ( 23.41677564524290744, 37.01856778792605240, -6.000000000000000000 ) ) ;
#1460 = CARTESIAN_POINT ( 'NONE',  ( -23.91865653299513994, -2.798222612723384906, 9.337377610831497421 ) ) ;
#1461 = CONICAL_SURFACE ( 'NONE', #9948, 4.699999872533999756, 0.7853981633972997312 ) ;
#1462 = CARTESIAN_POINT ( 'NONE',  ( 24.50000000000000711, -4.607483203864474852, 9.612698788763484714 ) ) ;
#1463 = CARTESIAN_POINT ( 'NONE',  ( -3.972370958142942055, 13.88120499530448271, 4.850339516680738150 ) ) ;
#1464 = CARTESIAN_POINT ( 'NONE',  ( -12.24999999999999645, 9.514185716142288030, -11.72205336956529820 ) ) ;
#1465 = AXIS2_PLACEMENT_3D ( 'NONE', #15450, #22836, #22601 ) ;
#1466 = CARTESIAN_POINT ( 'NONE',  ( -18.33732910583999853, -9.141853718868999223, 0.000000000000000000 ) ) ;
#1467 = EDGE_LOOP ( 'NONE', ( #22447, #19545, #3049 ) ) ;
#1468 = DIRECTION ( 'NONE',  ( 0.000000000000000000, -0.9999453485888588622, -0.01045465616390954186 ) ) ;
#1469 = CARTESIAN_POINT ( 'NONE',  ( 0.8491321808655799552, 24.60222989789001247, -4.128541458486335358 ) ) ;
#1470 = ORIENTED_EDGE ( 'NONE', *, *, #634, .T. ) ;
#1471 = CARTESIAN_POINT ( 'NONE',  ( -1.036892826754999941, 24.70947082776000059, -2.533142039532999767 ) ) ;
#1472 = DIRECTION ( 'NONE',  ( 0.000000000000000000, 1.000000000000000000, 0.000000000000000000 ) ) ;
#1473 = CARTESIAN_POINT ( 'NONE',  ( 11.09594815121217337, 0.9954690943758390809, -12.49999871279053920 ) ) ;
#1474 = CIRCLE ( 'NONE', #6092, 4.649999999999999467 ) ;
#1475 = CARTESIAN_POINT ( 'NONE',  ( 6.243179886996583328, 13.64542961362179518, -1.868502116970985671 ) ) ;
#1476 = DIRECTION ( 'NONE',  ( 0.000000000000000000, 0.000000000000000000, -1.000000000000000000 ) ) ;
#1477 = CARTESIAN_POINT ( 'NONE',  ( -2.500000000000000000, 24.00000000000000000, 8.181116922990998136E-14 ) ) ;
#1478 = ORIENTED_EDGE ( 'NONE', *, *, #19725, .T. ) ;
#1479 = CARTESIAN_POINT ( 'NONE',  ( -0.6543697108981929578, 30.00086340285666964, 2.434931691670791487 ) ) ;
#1480 = DIRECTION ( 'NONE',  ( 0.000000000000000000, 0.4408793407386908392, -0.8975663802247816347 ) ) ;
#1481 = CARTESIAN_POINT ( 'NONE',  ( 0.000000000000000000, 18.89999999999999858, 0.000000000000000000 ) ) ;
#1482 = PRODUCT_DEFINITION ( 'UNKNOWN', '', #2071, #16754 ) ;
#1483 = EDGE_LOOP ( 'NONE', ( #2128, #17775, #11631, #210 ) ) ;
#1484 = CARTESIAN_POINT ( 'NONE',  ( -20.18930073651999990, -0.1331888895339000123, -10.15414876350000029 ) ) ;
#1485 = CARTESIAN_POINT ( 'NONE',  ( 20.56670833333332382, -1.204281607287327249, -9.199063983722616911 ) ) ;
#1486 = CARTESIAN_POINT ( 'NONE',  ( 14.65490855118977720, 6.368553073539274578, -8.126428349890224112 ) ) ;
#1487 = DIRECTION ( 'NONE',  ( 0.000000000000000000, 0.000000000000000000, 1.000000000000000000 ) ) ;
#1488 = CARTESIAN_POINT ( 'NONE',  ( 23.90542041631999837, 10.75005818520000034, 3.477932657473000067 ) ) ;
#1489 = CARTESIAN_POINT ( 'NONE',  ( -1.755728607737000013, 30.01067697075000140, -1.271849504351999949 ) ) ;
#1490 = CARTESIAN_POINT ( 'NONE',  ( -22.45139694715554768, -7.393363156508755196, 5.681353437585703325 ) ) ;
#1491 = CARTESIAN_POINT ( 'NONE',  ( 2.320742031598997279, 11.86997853088999655, -4.174612069706000739 ) ) ;
#1492 = ORIENTED_EDGE ( 'NONE', *, *, #3306, .T. ) ;
#1493 = B_SPLINE_CURVE_WITH_KNOTS ( 'NONE', 3,
 ( #3469, #23790, #23909, #1993, #11208 ),
 .UNSPECIFIED., .F., .F.,
 ( 4, 1, 4 ),
 ( 0.000000000000000000, 0.5000000000000000000, 1.000000000000000000 ),
 .UNSPECIFIED. ) ;
#1494 = CONICAL_SURFACE ( 'NONE', #19680, 4.309401076758999416, 1.119376321708719590 ) ;
#1495 = DIRECTION ( 'NONE',  ( 1.000000000000000000, 0.000000000000000000, 0.000000000000000000 ) ) ;
#1496 = ORIENTED_EDGE ( 'NONE', *, *, #16640, .T. ) ;
#1497 = CARTESIAN_POINT ( 'NONE',  ( -0.1652120097165999946, 23.43138837836000121, -2.228042744016999865 ) ) ;
#1498 = CARTESIAN_POINT ( 'NONE',  ( -14.20256210577654166, -8.310917263278849276, 6.177374401935199266 ) ) ;
#1499 = EDGE_LOOP ( 'NONE', ( #18224, #22941 ) ) ;
#1500 = TOROIDAL_SURFACE ( 'NONE', #10383, 2.500000000000000000, 0.5500000000000000444 ) ;
#1501 = CIRCLE ( 'NONE', #4196, 3.000000000000000000 ) ;
#1502 = DIRECTION ( 'NONE',  ( -1.000000000000000000, 0.000000000000000000, 0.000000000000000000 ) ) ;
#1503 = CARTESIAN_POINT ( 'NONE',  ( 11.85409292834168049, -13.07924560384158852, -2.346130611933173071 ) ) ;
#1504 = CARTESIAN_POINT ( 'NONE',  ( 12.00000000000000355, 3.355345449857968454, -8.329183830964261404 ) ) ;
#1505 = COLOUR_RGB ( '', 0.08235294, 0.09019608, 0.10196078) ;
#1506 = DIRECTION ( 'NONE',  ( 0.000000000000000000, -1.000000000000000000, 0.000000000000000000 ) ) ;
#1507 = ORIENTED_EDGE ( 'NONE', *, *, #17841, .T. ) ;
#1508 = CARTESIAN_POINT ( 'NONE',  ( -11.62537363877000018, -0.5797963012832000329, 15.20738078243999958 ) ) ;
#1509 = AXIS2_PLACEMENT_3D ( 'NONE', #15833, #17544, #15703 ) ;
#1510 = CARTESIAN_POINT ( 'NONE',  ( 13.50000000000000178, 9.112083061060197053, -2.440520083675369101 ) ) ;
#1511 = CARTESIAN_POINT ( 'NONE',  ( 1.670409819843222898, 27.99999999999985079, -3.654390594373847723 ) ) ;
#1512 = ADVANCED_FACE ( 'NONE', ( #16470 ), #18202, .T. ) ;
#1513 = VERTEX_POINT ( 'NONE', #3427 ) ;
#1514 = CARTESIAN_POINT ( 'NONE',  ( 21.26450154976144802, -8.294907895047991531, -6.779548171067567353 ) ) ;
#1515 = B_SPLINE_CURVE_WITH_KNOTS ( 'NONE', 3,
 ( #765, #19176, #20996, #12044, #4290, #13598, #12163, #2584, #17737, #1142, #22919, #2839, #6462, #17235, #19053, #4780, #15413, #22800 ),
 .UNSPECIFIED., .F., .F.,
 ( 4, 2, 2, 2, 2, 2, 2, 2, 4 ),
 ( 0.000000000000000000, 0.1250000000000000278, 0.2500000000000000555, 0.3750000000000001110, 0.5000000000000001110, 0.6250000000000001110, 0.7500000000000000000, 0.8750000000000001110, 1.000000000000000000 ),
 .UNSPECIFIED. ) ;
#1516 = CARTESIAN_POINT ( 'NONE',  ( -13.99999999999999822, 1.087951517378483279, 9.623364086261211980 ) ) ;
#1517 = CARTESIAN_POINT ( 'NONE',  ( 17.31322874800178369, -4.549943461054996696, 9.392757792553869223 ) ) ;
#1518 = CARTESIAN_POINT ( 'NONE',  ( -17.00152607621999934, -4.780068549123999588, -9.988549307159999557 ) ) ;
#1519 = AXIS2_PLACEMENT_3D ( 'NONE', #892, #19439, #2849 ) ;
#1520 = CARTESIAN_POINT ( 'NONE',  ( -2.342248944605000105, 29.41754141063000105, 0.05822147085768999974 ) ) ;
#1521 = CARTESIAN_POINT ( 'NONE',  ( -12.50789737913000010, 5.572872693153001045, -7.876595158781000805 ) ) ;
#1522 = EDGE_CURVE ( 'NONE', #11301, #1186, #10138, .T. ) ;
#1523 = CARTESIAN_POINT ( 'NONE',  ( 1.058847381058417580, 29.93878768364113085, -1.884670918156025499 ) ) ;
#1524 = VERTEX_POINT ( 'NONE', #7268 ) ;
#1525 = CARTESIAN_POINT ( 'NONE',  ( 23.58884305931480796, -7.417893891498020587, 5.701350536648257972 ) ) ;
#1526 = CARTESIAN_POINT ( 'NONE',  ( 19.75239526568000059, -0.2837697319328000289, -11.37783472723000067 ) ) ;
#1527 = CARTESIAN_POINT ( 'NONE',  ( 19.76015484213748152, -5.065527522992182341, -9.203031659326928349 ) ) ;
#1528 = CARTESIAN_POINT ( 'NONE',  ( -0.8577166501281039412, 23.63976374042652395, -1.960334821351923384 ) ) ;
#1529 = AXIS2_PLACEMENT_3D ( 'NONE', #6973, #16287, #9266 ) ;
#1530 = ORIENTED_EDGE ( 'NONE', *, *, #10282, .F. ) ;
#1531 = CARTESIAN_POINT ( 'NONE',  ( 0.000000000000000000, 7.000000000000000000, 0.000000000000000000 ) ) ;
#1532 = CARTESIAN_POINT ( 'NONE',  ( 4.985850635142116793, 14.19104587639733772, -3.879869294806315594 ) ) ;
#1533 = CARTESIAN_POINT ( 'NONE',  ( -4.632032373251000479, 12.33312095925000307, -1.660520014003999512 ) ) ;
#1534 = ORIENTED_EDGE ( 'NONE', *, *, #2121, .F. ) ;
#1535 = CARTESIAN_POINT ( 'NONE',  ( 0.000000000000000000, 24.50000000000000000, -4.000000000000614619 ) ) ;
#1536 = EDGE_LOOP ( 'NONE', ( #8202, #9301 ) ) ;
#1537 = VECTOR ( 'NONE', #16304, 1000.000000000000114 ) ;
#1538 = FACE_OUTER_BOUND ( 'NONE', #11239, .T. ) ;
#1539 = CIRCLE ( 'NONE', #16992, 4.549999999999999822 ) ;
#1540 = CARTESIAN_POINT ( 'NONE',  ( 0.000000000000000000, 30.75000005827999772, 0.000000000000000000 ) ) ;
#1541 = EDGE_CURVE ( 'NONE', #13175, #5360, #5876, .T. ) ;
#1542 = ORIENTED_EDGE ( 'NONE', *, *, #20251, .T. ) ;
#1543 = CARTESIAN_POINT ( 'NONE',  ( -19.54076253787999562, 9.172736192578000214, 0.000000000000000000 ) ) ;
#1544 =( REPRESENTATION_RELATIONSHIP ('NONE','NONE', #13682, #22521 ) REPRESENTATION_RELATIONSHIP_WITH_TRANSFORMATION ( #21876 )SHAPE_REPRESENTATION_RELATIONSHIP( ) );
#1545 = CARTESIAN_POINT ( 'NONE',  ( -21.59814514390000184, -9.834866976764999436, 4.060023984597999736 ) ) ;
#1546 = CARTESIAN_POINT ( 'NONE',  ( 2.649999999999999911, 28.00000000000000000, 0.000000000000000000 ) ) ;
#1547 = CARTESIAN_POINT ( 'NONE',  ( -5.135907502119001045, 13.92753848266001349, -5.532842021099998675 ) ) ;
#1548 = CARTESIAN_POINT ( 'NONE',  ( -22.23430444492038305, 10.49227087223982302, -1.974901390299137915 ) ) ;
#1549 = CARTESIAN_POINT ( 'NONE',  ( -1.967423287079686611, 27.74445849415545595, -0.9951881276287170008 ) ) ;
#1550 = CARTESIAN_POINT ( 'NONE',  ( 2.870524099806999629, 27.65750240010000027, 0.05636985319957999591 ) ) ;
#1551 = CIRCLE ( 'NONE', #7323, 4.549999999999999822 ) ;
#1552 = EDGE_CURVE ( 'NONE', #22092, #13026, #22167, .T. ) ;
#1553 = CARTESIAN_POINT ( 'NONE',  ( 2.144633374660529501, 30.61889166568773391, -0.2565629783008914755 ) ) ;
#1554 = ORIENTED_EDGE ( 'NONE', *, *, #17032, .T. ) ;
#1555 = DIRECTION ( 'NONE',  ( 1.000000000000000000, 0.000000000000000000, 0.000000000000000000 ) ) ;
#1556 = CARTESIAN_POINT ( 'NONE',  ( 3.872051077439735423, 14.41258966728797120, 4.746043954005092047 ) ) ;
#1557 = CARTESIAN_POINT ( 'NONE',  ( -1.259486242684000112, 26.26869850838000175, 1.884954223019000175 ) ) ;
#1558 = B_SPLINE_CURVE_WITH_KNOTS ( 'NONE', 3,
 ( #5315, #8955, #20647, #22575, #16323, #23824, #3392, #12586, #7235, #20210, #22023, #4056, #5981, #11451, #18825, #5436, #2232, #9182 ),
 .UNSPECIFIED., .F., .F.,
 ( 4, 2, 2, 2, 2, 2, 2, 2, 4 ),
 ( 0.000000000000000000, 0.1249999999999999167, 0.2499999999999998890, 0.3749999999999998335, 0.4999999999999998890, 0.6249999999999998890, 0.7499999999999998890, 0.8750000000000000000, 1.000000000000000000 ),
 .UNSPECIFIED. ) ;
#1559 = CARTESIAN_POINT ( 'NONE',  ( 2.252185756629999869, 28.21021896306000087, 0.4021892318948999678 ) ) ;
#1560 = CIRCLE ( 'NONE', #5795, 1.999999992708000773 ) ;
#1561 = CARTESIAN_POINT ( 'NONE',  ( 1.472357546044718912, 11.57346035306418663, 4.589515119174757629 ) ) ;
#1562 = ORIENTED_EDGE ( 'NONE', *, *, #6602, .F. ) ;
#1563 = CARTESIAN_POINT ( 'NONE',  ( 17.73233333333332595, 4.596309454924390359, 7.974412893977484096 ) ) ;
#1564 = CARTESIAN_POINT ( 'NONE',  ( 4.801955413365184278, 12.43156791562425489, -0.6979716084022052902 ) ) ;
#1565 = CARTESIAN_POINT ( 'NONE',  ( -10.53807879897562394, 15.50632097202035098, 1.406271040994186761 ) ) ;
#1566 = CARTESIAN_POINT ( 'NONE',  ( -21.20359587121333433, 8.052249294577444871, 4.641171550773364629 ) ) ;
#1567 = ORIENTED_EDGE ( 'NONE', *, *, #2903, .F. ) ;
#1568 = EDGE_CURVE ( 'NONE', #20019, #13096, #454, .T. ) ;
#1569 = EDGE_CURVE ( 'NONE', #12723, #13227, #7816, .T. ) ;
#1570 = CARTESIAN_POINT ( 'NONE',  ( -11.00000000000000000, 10.59999999999999964, 0.000000000000000000 ) ) ;
#1571 = CYLINDRICAL_SURFACE ( 'NONE', #15011, 2.673746900119611247 ) ;
#1572 = CARTESIAN_POINT ( 'NONE',  ( 11.96718892131000089, -1.481964887125999830, -9.481920936164000224 ) ) ;
#1573 = CARTESIAN_POINT ( 'NONE',  ( 18.45432512885125576, 9.931295749172702969, -3.157890530097379411 ) ) ;
#1574 = CARTESIAN_POINT ( 'NONE',  ( -0.6543697108981929578, 29.20086340285667248, 2.434931691670791487 ) ) ;
#1575 = CARTESIAN_POINT ( 'NONE',  ( 2.300329438417999750, 29.07312603901999992, -0.4386776513298999980 ) ) ;
#1576 = CARTESIAN_POINT ( 'NONE',  ( 66.60588651278291650, 37.01856778792605240, 1.000000000000000000 ) ) ;
#1577 = CARTESIAN_POINT ( 'NONE',  ( 18.51344355829000321, 6.966878364870000340, -12.06698729810999993 ) ) ;
#1578 = B_SPLINE_CURVE_WITH_KNOTS ( 'NONE', 3,
 ( #16341, #7138, #13063, #20339, #3870 ),
 .UNSPECIFIED., .F., .F.,
 ( 4, 1, 4 ),
 ( 0.000000000000000000, 0.5000000000000000000, 1.000000000000000000 ),
 .UNSPECIFIED. ) ;
#1579 = ORIENTED_EDGE ( 'NONE', *, *, #8821, .T. ) ;
#1580 = FACE_OUTER_BOUND ( 'NONE', #8119, .T. ) ;
#1581 = CARTESIAN_POINT ( 'NONE',  ( 19.86475848803999966, -8.290923745122999122, -6.795056182818000501 ) ) ;
#1582 = EDGE_CURVE ( 'NONE', #9355, #6055, #19428, .T. ) ;
#1583 = CARTESIAN_POINT ( 'NONE',  ( 2.500000000000000000, 29.19999999999999929, 0.000000000000000000 ) ) ;
#1584 = EDGE_CURVE ( 'NONE', #11323, #18038, #22501, .T. ) ;
#1585 = CARTESIAN_POINT ( 'NONE',  ( 13.80672594031167399, -10.34511788736346638, 0.1683342567789284094 ) ) ;
#1586 = CARTESIAN_POINT ( 'NONE',  ( -4.277841172294765570, 13.62415523807033324, 4.947054612845048993 ) ) ;
#1587 = CARTESIAN_POINT ( 'NONE',  ( -2.715077639162999823, 11.83540306990998481, 4.154853624383998856 ) ) ;
#1588 = CARTESIAN_POINT ( 'NONE',  ( -12.25000000000000178, 8.353912356140339668, -12.24351521210916438 ) ) ;
#1589 = VERTEX_POINT ( 'NONE', #1946 ) ;
#1590 = DIRECTION ( 'NONE',  ( 0.000000000000000000, -1.000000000000000000, 0.000000000000000000 ) ) ;
#1591 = CARTESIAN_POINT ( 'NONE',  ( 1.800000000175999926, 13.00000000000000000, 1.081665382745000015 ) ) ;
#1592 = ORIENTED_EDGE ( 'NONE', *, *, #22403, .F. ) ;
#1593 = CARTESIAN_POINT ( 'NONE',  ( -2.372070577900000199, 23.90733340193000345, -0.9226943487805999711 ) ) ;
#1594 = FACE_OUTER_BOUND ( 'NONE', #3534, .T. ) ;
#1595 = CARTESIAN_POINT ( 'NONE',  ( 4.146132389986815880, 13.37806292782055984, 5.418534502940187458 ) ) ;
#1596 = CARTESIAN_POINT ( 'NONE',  ( 12.50448233770999984, 13.93375672974000068, 0.4328756433527000680 ) ) ;
#1597 = CARTESIAN_POINT ( 'NONE',  ( 13.50000000000000000, -4.865356088987999428, 9.073685197596999430 ) ) ;
#1598 = CARTESIAN_POINT ( 'NONE',  ( 8.124934037954998800, 14.44999999999999929, 0.000000000000000000 ) ) ;
#1599 = ORIENTED_EDGE ( 'NONE', *, *, #23855, .T. ) ;
#1600 = CARTESIAN_POINT ( 'NONE',  ( -15.35172225070999907, -1.839441420978000119, 9.553397381538999866 ) ) ;
#1601 = CONICAL_SURFACE ( 'NONE', #17442, 4.309401076758999416, 1.119376321708719590 ) ;
#1602 = CARTESIAN_POINT ( 'NONE',  ( 60.61494135913342518, 27.01856778792605240, 2.673746900119611247 ) ) ;
#1603 = DIRECTION ( 'NONE',  ( 1.000000000000000000, 0.000000000000000000, 0.000000000000000000 ) ) ;
#1604 = ORIENTED_EDGE ( 'NONE', *, *, #180, .T. ) ;
#1605 = CARTESIAN_POINT ( 'NONE',  ( -10.38832047382276613, 15.62395172623501871, -1.271871094456791473 ) ) ;
#1606 = CARTESIAN_POINT ( 'NONE',  ( -2.032167282806999875, 24.44908585634999909, -0.6853045129910999567 ) ) ;
#1607 = CARTESIAN_POINT ( 'NONE',  ( 14.77055141664746429, 9.043857732850597131, -4.985902765646755164 ) ) ;
#1608 = CARTESIAN_POINT ( 'NONE',  ( 4.000000000000117240, 24.49999999999975486, 0.1904558375517787505 ) ) ;
#1609 = CARTESIAN_POINT ( 'NONE',  ( 18.98657778229999948, -9.749946538104000027, 5.437902738275999681 ) ) ;
#1610 = CARTESIAN_POINT ( 'NONE',  ( -2.336652659577999724, 30.76694896736999851, -0.3346041500006000091 ) ) ;
#1611 = CARTESIAN_POINT ( 'NONE',  ( 13.69869376140666972, 8.478391648451442109, -3.082568484730727310 ) ) ;
#1612 = CARTESIAN_POINT ( 'NONE',  ( 4.220193709370997581, 12.42420947506999873, -2.355922916967998049 ) ) ;
#1613 = CARTESIAN_POINT ( 'NONE',  ( 2.100000000000000089, 28.30000000000000071, 0.000000000000000000 ) ) ;
#1614 = ORIENTED_EDGE ( 'NONE', *, *, #12057, .T. ) ;
#1615 = CARTESIAN_POINT ( 'NONE',  ( -2.999999998489146336, 15.10000000000041176, 8.997179835138123378E-10 ) ) ;
#1616 = ORIENTED_EDGE ( 'NONE', *, *, #7937, .F. ) ;
#1617 = CARTESIAN_POINT ( 'NONE',  ( -4.625000000000000000, 13.00000000000000000, 0.000000000000000000 ) ) ;
#1618 = CARTESIAN_POINT ( 'NONE',  ( 17.27883333333331706, 7.964244026804120580, -4.590448486402081585 ) ) ;
#1619 = DIRECTION ( 'NONE',  ( 0.000000000000000000, 1.000000000000000000, 0.000000000000000000 ) ) ;
#1620 = CARTESIAN_POINT ( 'NONE',  ( 18.30212984639999974, 10.73999106964999939, 2.881100424796000148 ) ) ;
#1621 = ORIENTED_EDGE ( 'NONE', *, *, #21569, .T. ) ;
#1622 = CARTESIAN_POINT ( 'NONE',  ( -9.087185065846002274, 6.105045399203000045, -13.55681854251999852 ) ) ;
#1623 = CARTESIAN_POINT ( 'NONE',  ( 13.49999999999999822, 9.355385045509903463, 2.879371244180602307 ) ) ;
#1624 = FACE_OUTER_BOUND ( 'NONE', #21156, .T. ) ;
#1625 = ORIENTED_EDGE ( 'NONE', *, *, #4322, .T. ) ;
#1626 = CARTESIAN_POINT ( 'NONE',  ( 23.38235175880183192, 1.726590010014731336, -10.45918579154710315 ) ) ;
#1627 = CARTESIAN_POINT ( 'NONE',  ( 12.51792796885999870, -13.93375672974000068, 0.7216006907722000152 ) ) ;
#1628 = CARTESIAN_POINT ( 'NONE',  ( 16.10298205229174329, -5.908803289076222320, -8.512465605292881321 ) ) ;
#1629 = CARTESIAN_POINT ( 'NONE',  ( -18.82862077250666744, 1.198189225339994612, 9.154461231320610182 ) ) ;
#1630 = VECTOR ( 'NONE', #19185, 1000.000000000000114 ) ;
#1631 = CARTESIAN_POINT ( 'NONE',  ( 2.107129814228999809, 29.86750533736999813, -0.5904572975527000445 ) ) ;
#1632 = CARTESIAN_POINT ( 'NONE',  ( -13.11728842303999976, -9.638936811879000643, -0.7309380707209000017 ) ) ;
#1633 = CARTESIAN_POINT ( 'NONE',  ( 1.813637125157641083, 29.87718600260956947, -1.176169980081204436 ) ) ;
#1634 = ORIENTED_EDGE ( 'NONE', *, *, #2422, .F. ) ;
#1635 = CARTESIAN_POINT ( 'NONE',  ( 23.70216531585290909, -8.985547010004388824, 2.405992734474589945 ) ) ;
#1636 = CARTESIAN_POINT ( 'NONE',  ( 22.51237305742672135, 4.065799934601714405, 9.766473785554790510 ) ) ;
#1637 = CARTESIAN_POINT ( 'NONE',  ( -12.48243343204000055, 6.965111533508000718, -5.686492047758000545 ) ) ;
#1638 = AXIS2_PLACEMENT_3D ( 'NONE', #20243, #3647, #20477 ) ;
#1639 = ORIENTED_EDGE ( 'NONE', *, *, #2556, .F. ) ;
#1640 = EDGE_CURVE ( 'NONE', #11953, #23400, #3577, .T. ) ;
#1641 = DIRECTION ( 'NONE',  ( 0.000000000000000000, -1.000000000000000000, 0.000000000000000000 ) ) ;
#1642 = CARTESIAN_POINT ( 'NONE',  ( 4.854249925572221791, 14.55265595715461124, -3.782643825661391457 ) ) ;
#1643 = CARTESIAN_POINT ( 'NONE',  ( -4.263501161146997731, 12.20307014857999839, -2.457753744994997547 ) ) ;
#1644 = ORIENTED_EDGE ( 'NONE', *, *, #4507, .T. ) ;
#1645 = CARTESIAN_POINT ( 'NONE',  ( 0.000000000000000000, 9.050044887908999414, -1.949955127985000258 ) ) ;
#1646 = ORIENTED_EDGE ( 'NONE', *, *, #7863, .T. ) ;
#1647 = CARTESIAN_POINT ( 'NONE',  ( -1.999167105995441673, 28.31753006952333607, 1.536366799937297856 ) ) ;
#1648 = CARTESIAN_POINT ( 'NONE',  ( 1.259047450927256895, 29.86666666666666359, 2.184465970885639763 ) ) ;
#1649 = EDGE_CURVE ( 'NONE', #13003, #12335, #9333, .T. ) ;
#1650 = ORIENTED_EDGE ( 'NONE', *, *, #10005, .T. ) ;
#1651 = CARTESIAN_POINT ( 'NONE',  ( -12.49414447734999989, 6.965344330034999309, -5.686682108691999638 ) ) ;
#1652 = CARTESIAN_POINT ( 'NONE',  ( -23.47319277894999701, -9.624513788245998569, -3.290287683043000122 ) ) ;
#1653 = CARTESIAN_POINT ( 'NONE',  ( -18.60511922971000232, -7.342831292577000291, 6.519673310378999886 ) ) ;
#1654 = CARTESIAN_POINT ( 'NONE',  ( -6.378350646088002840, 15.10313706270000189, -3.204455250576998981 ) ) ;
#1655 = LINE ( 'NONE', #18481, #14678 ) ;
#1656 = CARTESIAN_POINT ( 'NONE',  ( -0.6576427108141560396, 26.84341933061397611, -2.107288224371474783 ) ) ;
#1657 = CARTESIAN_POINT ( 'NONE',  ( 2.387212940976999764, 28.53500240009999800, -1.595084814687000030 ) ) ;
#1658 = CARTESIAN_POINT ( 'NONE',  ( 2.001789734241726570, 30.65294125138512626, -0.8114744869051462306 ) ) ;
#1659 = ORIENTED_EDGE ( 'NONE', *, *, #14309, .F. ) ;
#1660 = CARTESIAN_POINT ( 'NONE',  ( -18.33732910583999853, -9.141853718868999223, 0.000000000000000000 ) ) ;
#1661 = DIRECTION ( 'NONE',  ( 0.000000000000000000, 1.000000000000000000, 0.000000000000000000 ) ) ;
#1662 = CARTESIAN_POINT ( 'NONE',  ( 13.93567587029640364, 7.873185683027793758, -4.525993401469360577 ) ) ;
#1663 = CONICAL_SURFACE ( 'NONE', #21391, 2.249999993279999888, 0.7853981633972997312 ) ;
#1664 = EDGE_CURVE ( 'NONE', #3791, #12959, #10926, .T. ) ;
#1665 = CARTESIAN_POINT ( 'NONE',  ( 0.04491825056511999925, 27.23521896306000301, 2.287373719275000106 ) ) ;
#1666 = CARTESIAN_POINT ( 'NONE',  ( 2.899766981581773706, 11.83721411937113821, 3.858556422892893245 ) ) ;
#1667 = EDGE_LOOP ( 'NONE', ( #1625, #4186, #23393, #4526 ) ) ;
#1668 = CARTESIAN_POINT ( 'NONE',  ( 0.4089070776637447335, 11.48994554096019982, -4.794126951967982997 ) ) ;
#1669 = CARTESIAN_POINT ( 'NONE',  ( 24.27836688955406430, 7.477364734544921454, -6.207148011325140047 ) ) ;
#1670 = DIRECTION ( 'NONE',  ( 0.000000000000000000, 1.000000000000000000, 0.000000000000000000 ) ) ;
#1671 = EDGE_LOOP ( 'NONE', ( #5379, #9334, #2085, #16002 ) ) ;
#1672 = ADVANCED_FACE ( 'NONE', ( #11276 ), #14887, .F. ) ;
#1673 = CARTESIAN_POINT ( 'NONE',  ( -2.500000000000000000, 24.00000000000000000, 8.181116922990998136E-14 ) ) ;
#1674 = CARTESIAN_POINT ( 'NONE',  ( -6.637070260807000466, 27.93157662065900126, 1.000000000000000000 ) ) ;
#1675 = CARTESIAN_POINT ( 'NONE',  ( 17.25862658530999738, -10.23584709072999921, -0.4386478486912999686 ) ) ;
#1676 = CARTESIAN_POINT ( 'NONE',  ( 18.58956004406604023, 10.30724957857451329, 1.570066827172868607 ) ) ;
#1677 = UNCERTAINTY_MEASURE_WITH_UNIT (LENGTH_MEASURE( 1.000000000000000082E-05 ), #20239, 'distance_accuracy_value', 'NONE');
#1678 = CARTESIAN_POINT ( 'NONE',  ( 2.500000000000001776, 29.41753006952333394, 0.3272492347489266429 ) ) ;
#1679 = CARTESIAN_POINT ( 'NONE',  ( -0.7692266288049000034, 29.49712917223999753, 2.008491639871999634 ) ) ;
#1680 = CARTESIAN_POINT ( 'NONE',  ( -12.50349985809999964, 6.524880561163000081, -6.187457173207999261 ) ) ;
#1681 = CARTESIAN_POINT ( 'NONE',  ( 13.49999999999999822, -8.267279161049540193, 5.671028086302140281 ) ) ;
#1682 = ORIENTED_EDGE ( 'NONE', *, *, #28, .T. ) ;
#1683 = AXIS2_PLACEMENT_3D ( 'NONE', #15512, #19281, #10081 ) ;
#1684 = EDGE_CURVE ( 'NONE', #14929, #16467, #10917, .T. ) ;
#1685 = CARTESIAN_POINT ( 'NONE',  ( 4.835177208035999818, 0.000000000000000000, 0.000000000000000000 ) ) ;
#1686 = CARTESIAN_POINT ( 'NONE',  ( 23.13443595893999927, -10.50750968058000012, -4.259898950046999921 ) ) ;
#1687 = LINE ( 'NONE', #9076, #350 ) ;
#1688 = CARTESIAN_POINT ( 'NONE',  ( 13.69521714869160967, -9.517818908541695322, 4.057451185538291760 ) ) ;
#1689 = FACE_BOUND ( 'NONE', #22379, .T. ) ;
#1690 = CARTESIAN_POINT ( 'NONE',  ( 7.500000000000000000, -10.00000000000000000, 0.000000000000000000 ) ) ;
#1691 = CARTESIAN_POINT ( 'NONE',  ( 0.2865205186993326492, 29.18676986812987195, -2.140916946558517608 ) ) ;
#1692 = EDGE_CURVE ( 'NONE', #8826, #10857, #17559, .T. ) ;
#1693 = CARTESIAN_POINT ( 'NONE',  ( -23.31326413257000141, 3.475863815851999661, 10.58457578842000046 ) ) ;
#1694 = EDGE_LOOP ( 'NONE', ( #8143, #22988, #19930, #23524, #16581, #9411, #11945, #14595, #20479, #9039, #14531 ) ) ;
#1695 = EDGE_CURVE ( 'NONE', #11307, #14835, #4740, .T. ) ;
#1696 = CARTESIAN_POINT ( 'NONE',  ( -3.999999999999999112, 26.41068681084913194, 1.228746328088897721 ) ) ;
#1697 = ORIENTED_EDGE ( 'NONE', *, *, #21953, .F. ) ;
#1698 = CARTESIAN_POINT ( 'NONE',  ( -2.120220590722000420, 25.36855084940000182, 0.4191826807252999609 ) ) ;
#1699 = CARTESIAN_POINT ( 'NONE',  ( -2.499999999999999556, 28.01666666666666927, 0.3272492347489423525 ) ) ;
#1700 = CARTESIAN_POINT ( 'NONE',  ( 11.43887872963225938, 3.075720902665963763, -12.49994001780840058 ) ) ;
#1701 = FACE_OUTER_BOUND ( 'NONE', #726, .T. ) ;
#1702 = CARTESIAN_POINT ( 'NONE',  ( 2.500000000000000000, 27.59999999999999787, 0.000000000000000000 ) ) ;
#1703 = CARTESIAN_POINT ( 'NONE',  ( 14.62612658531000243, 9.561303730670999812, 3.483288127948000135 ) ) ;
#1704 = SHAPE_REPRESENTATION_RELATIONSHIP ( 'NONE' , 'NONE' ,  #14475, #674 ) ;
#1705 = EDGE_CURVE ( 'NONE', #13340, #18875, #16390, .T. ) ;
#1706 = ORIENTED_EDGE ( 'NONE', *, *, #13562, .F. ) ;
#1707 = CARTESIAN_POINT ( 'NONE',  ( -18.13088126894000141, 1.446686056264999920E-14, 0.000000000000000000 ) ) ;
#1708 = CARTESIAN_POINT ( 'NONE',  ( -1.664359855051821491, 26.21279260321131588, 1.307626407210986219 ) ) ;
#1709 = LINE ( 'NONE', #11035, #17167 ) ;
#1710 = ORIENTED_EDGE ( 'NONE', *, *, #14895, .T. ) ;
#1711 = CARTESIAN_POINT ( 'NONE',  ( -10.58090218245767389, 15.47935404656033853, -1.445406436927922700 ) ) ;
#1712 = CARTESIAN_POINT ( 'NONE',  ( -0.5089225745698999770, 24.32100362754999878, -2.083349215147999978 ) ) ;
#1713 = CARTESIAN_POINT ( 'NONE',  ( 14.54031634975408949, 2.702827404106709075, -9.961777166465550337 ) ) ;
#1714 = AXIS2_PLACEMENT_3D ( 'NONE', #10682, #18068, #1476 ) ;
#1715 = CARTESIAN_POINT ( 'NONE',  ( -17.72676253787999912, 9.126185377371999863, 0.000000000000000000 ) ) ;
#1716 = CARTESIAN_POINT ( 'NONE',  ( 20.93174364276999810, -5.383988185498999712, 9.840443131421999112 ) ) ;
#1717 = CARTESIAN_POINT ( 'NONE',  ( 0.3968543755643999527, 29.86705919954999899, -2.131358888218999770 ) ) ;
#1718 = CARTESIAN_POINT ( 'NONE',  ( 14.09937895178651956, 4.578329686716531732, 7.785341728062208588 ) ) ;
#1719 = CARTESIAN_POINT ( 'NONE',  ( -3.588253153925999417, 12.21993382980000931, -3.223409665062000329 ) ) ;
#1720 = B_SPLINE_CURVE_WITH_KNOTS ( 'NONE', 3,
 ( #19359, #2765, #930, #17904, #10396, #17787 ),
 .UNSPECIFIED., .F., .F.,
 ( 4, 2, 4 ),
 ( 0.7901839888852105753, 0.8950919944426052322, 1.000000000000000000 ),
 .UNSPECIFIED. ) ;
#1721 = SURFACE_STYLE_USAGE ( .BOTH. , #18318 ) ;
#1722 = EDGE_CURVE ( 'NONE', #1842, #7244, #14041, .T. ) ;
#1723 = ORIENTED_EDGE ( 'NONE', *, *, #16063, .F. ) ;
#1724 = EDGE_CURVE ( 'NONE', #1220, #14845, #1080, .T. ) ;
#1725 = AXIS2_PLACEMENT_3D ( 'NONE', #21645, #5061, #12442 ) ;
#1726 = CARTESIAN_POINT ( 'NONE',  ( -14.69275774687465486, -4.229081981004126689, -8.019797593851203388 ) ) ;
#1727 = CARTESIAN_POINT ( 'NONE',  ( 24.49999999999999289, -10.07254353310004369, -1.427226065814861000 ) ) ;
#1728 = ORIENTED_EDGE ( 'NONE', *, *, #8958, .F. ) ;
#1729 = CARTESIAN_POINT ( 'NONE',  ( 0.000000000000000000, 7.049999902385000183, -1.449999902385000095 ) ) ;
#1730 = CARTESIAN_POINT ( 'NONE',  ( 11.55284350194278531, -12.59061462088587646, -3.192208964457393439 ) ) ;
#1731 = DIRECTION ( 'NONE',  ( -0.000000000000000000, 1.000000000000000000, 0.000000000000000000 ) ) ;
#1732 = CIRCLE ( 'NONE', #9456, 4.000000000000000000 ) ;
#1733 = CARTESIAN_POINT ( 'NONE',  ( 24.32802197706165259, 3.549421024388790258, -12.50000000000000355 ) ) ;
#1734 = CARTESIAN_POINT ( 'NONE',  ( -15.31190575492827044, -4.623917834005626837, -9.292808272911738499 ) ) ;
#1735 = B_SPLINE_CURVE_WITH_KNOTS ( 'NONE', 3,
 ( #5787, #11487, #16682, #90, #18862, #3974 ),
 .UNSPECIFIED., .F., .F.,
 ( 4, 2, 4 ),
 ( 0.002503788684009304773, 0.003059594342613334954, 0.003615400001217365135 ),
 .UNSPECIFIED. ) ;
#1736 = CARTESIAN_POINT ( 'NONE',  ( 2.361836001938000251, 25.62256359724000276, -0.7160459369172998967 ) ) ;
#1737 = EDGE_CURVE ( 'NONE', #1360, #17036, #8351, .T. ) ;
#1738 = ORIENTED_EDGE ( 'NONE', *, *, #8654, .T. ) ;
#1739 = CIRCLE ( 'NONE', #12188, 1.000000000000000888 ) ;
#1740 = CARTESIAN_POINT ( 'NONE',  ( -9.596297565846001021, -14.72535623507000047, 2.054682120933999823 ) ) ;
#1741 = CARTESIAN_POINT ( 'NONE',  ( 13.50000000000000000, 9.582599390072616075, 0.7345775502715846672 ) ) ;
#1742 = FACE_OUTER_BOUND ( 'NONE', #7598, .T. ) ;
#1743 = EDGE_LOOP ( 'NONE', ( #21400, #18889, #3660, #23863 ) ) ;
#1744 = CARTESIAN_POINT ( 'NONE',  ( 22.67640168912134513, -8.018325136500161321, 6.902805651056266534 ) ) ;
#1745 = DIRECTION ( 'NONE',  ( -1.000000000000000000, 0.000000000000000000, 0.000000000000000000 ) ) ;
#1746 = CARTESIAN_POINT ( 'NONE',  ( 16.01635173159208492, -8.104727441204580884, -6.451229416688261331 ) ) ;
#1747 = CARTESIAN_POINT ( 'NONE',  ( 2.100000000000000089, 18.10000000000000142, 2.368341633917999944E-10 ) ) ;
#1748 = CARTESIAN_POINT ( 'NONE',  ( -1.865383466706000082, 31.09043468882000028, 0.9086832089919000266 ) ) ;
#1749 = AXIS2_PLACEMENT_3D ( 'NONE', #21319, #2915, #23114 ) ;
#1750 = CARTESIAN_POINT ( 'NONE',  ( -17.58615607838000372, 9.339993809354998788, 2.937842867551999859 ) ) ;
#1751 = CARTESIAN_POINT ( 'NONE',  ( 2.136626277416635133, 29.82246383866652195, -0.3158569418315477217 ) ) ;
#1752 = ORIENTED_EDGE ( 'NONE', *, *, #16515, .F. ) ;
#1753 = CARTESIAN_POINT ( 'NONE',  ( 2.112124071471999986, 24.20052506214999966, 0.5457312241595999591 ) ) ;
#1754 = CARTESIAN_POINT ( 'NONE',  ( 22.22863922079730514, 10.51474377966081875, 2.086151727073547679 ) ) ;
#1755 = FACE_OUTER_BOUND ( 'NONE', #103, .T. ) ;
#1756 = ORIENTED_EDGE ( 'NONE', *, *, #16140, .T. ) ;
#1757 = CARTESIAN_POINT ( 'NONE',  ( -0.1513776656675359655, 24.53216460021022272, -2.367835399791780482 ) ) ;
#1758 = CARTESIAN_POINT ( 'NONE',  ( -6.378247030388997985, 15.10307864196000516, 3.204776768353000183 ) ) ;
#1759 = B_SPLINE_CURVE_WITH_KNOTS ( 'NONE', 3,
 ( #22778, #2936, #13822, #2696 ),
 .UNSPECIFIED., .F., .F.,
 ( 4, 4 ),
 ( 3.110165528588429006E-14, 0.0001520356277385664402 ),
 .UNSPECIFIED. ) ;
#1760 = CARTESIAN_POINT ( 'NONE',  ( 2.361827492105001536, 11.73717613017002037, -4.198437883487004640 ) ) ;
#1761 = VERTEX_POINT ( 'NONE', #21434 ) ;
#1762 = CARTESIAN_POINT ( 'NONE',  ( 15.56043875731000092, 5.001549981505999831, -7.700678710662999471 ) ) ;
#1763 = EDGE_LOOP ( 'NONE', ( #22179, #4490, #19938 ) ) ;
#1764 = VECTOR ( 'NONE', #4364, 1000.000000000000000 ) ;
#1765 = CARTESIAN_POINT ( 'NONE',  ( -2.184465970885638875, 28.30086340285666680, 1.259047450927259559 ) ) ;
#1766 = ITEM_DEFINED_TRANSFORMATION ( 'NONE', 'NONE', #23714,  #4390 ) ;
#1767 = CARTESIAN_POINT ( 'NONE',  ( -14.50000017815840891, 0.2596243778658171020, -12.49999897408938310 ) ) ;
#1768 = ORIENTED_EDGE ( 'NONE', *, *, #4821, .T. ) ;
#1769 = CARTESIAN_POINT ( 'NONE',  ( 1.999582798912397763, 24.48329780672474598, -1.535796015288176664 ) ) ;
#1770 = CARTESIAN_POINT ( 'NONE',  ( -25.34824041399999928, -4.583299861329000358, -7.994677941742001082 ) ) ;
#1771 = EDGE_CURVE ( 'NONE', #6372, #15650, #8993, .T. ) ;
#1772 = CARTESIAN_POINT ( 'NONE',  ( 12.12543434885914095, -8.197779943747480758, -10.80110243434621431 ) ) ;
#1773 = CARTESIAN_POINT ( 'NONE',  ( -5.600699945962000825, 15.08715837589000053, -2.809455428781000297 ) ) ;
#1774 = CARTESIAN_POINT ( 'NONE',  ( -23.85561736702028313, 9.397789499121957491, 4.882708127867132042 ) ) ;
#1775 = CARTESIAN_POINT ( 'NONE',  ( -2.020216954725641667, 27.05542854569362632, 0.8542913370163738307 ) ) ;
#1776 = CARTESIAN_POINT ( 'NONE',  ( 2.030158388880999976, 27.56000240010000013, 2.030158388880999976 ) ) ;
#1777 = CARTESIAN_POINT ( 'NONE',  ( -0.9358744650684699407, 29.91068681084918879, 4.078474779182606369 ) ) ;
#1778 = ORIENTED_EDGE ( 'NONE', *, *, #22021, .T. ) ;
#1779 = CARTESIAN_POINT ( 'NONE',  ( 0.000000000000000000, 21.87500000000000000, 0.000000000000000000 ) ) ;
#1780 = CARTESIAN_POINT ( 'NONE',  ( 14.21567657034085208, 8.191001517356450989, 3.937144643937185773 ) ) ;
#1781 = VECTOR ( 'NONE', #5397, 1000.000000000000000 ) ;
#1782 = CARTESIAN_POINT ( 'NONE',  ( 5.818132659865536738, 14.45536608084069208, -1.914417212635753929 ) ) ;
#1783 = CARTESIAN_POINT ( 'NONE',  ( 2.189073617939000016, 25.87021896306000102, -0.6636689712801000507 ) ) ;
#1784 = CARTESIAN_POINT ( 'NONE',  ( -2.123501712390408525, 30.87060775419617897, 0.1583979370652605911 ) ) ;
#1785 = CARTESIAN_POINT ( 'NONE',  ( 4.254626796002882294, 12.23359600459727758, 2.313684877474057267 ) ) ;
#1786 = EDGE_LOOP ( 'NONE', ( #15697, #16611, #15498, #7312, #19793, #10078, #15131, #16394, #6992, #18684 ) ) ;
#1787 = CARTESIAN_POINT ( 'NONE',  ( -4.339621077386181192, 12.26288397286404575, -2.157489521576238634 ) ) ;
#1788 = CARTESIAN_POINT ( 'NONE',  ( 3.000000000000000000, 19.09999999999999787, 0.000000000000000000 ) ) ;
#1789 = CARTESIAN_POINT ( 'NONE',  ( 4.835083642289389694, 12.44448910615697912, 0.3758261001295359338 ) ) ;
#1790 = ORIENTED_EDGE ( 'NONE', *, *, #9816, .F. ) ;
#1791 = DIRECTION ( 'NONE',  ( 0.5000000000000169864, 0.000000000000000000, -0.8660254037844288266 ) ) ;
#1792 = DIRECTION ( 'NONE',  ( 0.000000000000000000, 0.000000000000000000, 1.000000000000000000 ) ) ;
#1793 = CIRCLE ( 'NONE', #4902, 3.000000000000000000 ) ;
#1794 = CONICAL_SURFACE ( 'NONE', #8852, 1.949955127985000258, 0.7853751480324476786 ) ;
#1795 = CARTESIAN_POINT ( 'NONE',  ( 14.73581408531000037, 7.589869243736000470, 6.782654363299000622 ) ) ;
#1796 = CARTESIAN_POINT ( 'NONE',  ( 18.45416163448745195, 9.929482224075606211, -3.163580258347401308 ) ) ;
#1797 = EDGE_CURVE ( 'NONE', #12884, #21421, #1941, .T. ) ;
#1798 = CARTESIAN_POINT ( 'NONE',  ( 2.184465970885649089, 29.36753006952332967, 1.259047450927240241 ) ) ;
#1799 = FACE_OUTER_BOUND ( 'NONE', #14293, .T. ) ;
#1800 = CARTESIAN_POINT ( 'NONE',  ( 0.000000000000000000, 14.90000000000000036, 0.000000000000000000 ) ) ;
#1801 = CARTESIAN_POINT ( 'NONE',  ( 13.50000000000000355, -8.034537072252554424, 6.023462719563941192 ) ) ;
#1802 = ORIENTED_EDGE ( 'NONE', *, *, #23005, .F. ) ;
#1803 = FACE_OUTER_BOUND ( 'NONE', #1499, .T. ) ;
#1804 = CARTESIAN_POINT ( 'NONE',  ( 24.82213334836999863, -5.577735010582999919, 8.534839029212999861 ) ) ;
#1805 = CARTESIAN_POINT ( 'NONE',  ( -4.000000000000000000, 24.50000000000000000, -2.309401076759000304 ) ) ;
#1806 = AXIS2_PLACEMENT_3D ( 'NONE', #5878, #20902, #13149 ) ;
#1807 = DIRECTION ( 'NONE',  ( 0.000000000000000000, 1.000000000000000000, 0.000000000000000000 ) ) ;
#1808 = CARTESIAN_POINT ( 'NONE',  ( 24.50000000000000711, 2.053173317924622765, 10.18216561726737091 ) ) ;
#1809 = CARTESIAN_POINT ( 'NONE',  ( -4.776861987225999862, 12.47838630334000065, -0.1510726511063999189 ) ) ;
#1810 = CARTESIAN_POINT ( 'NONE',  ( -0.2595857393297835713, 29.21926038359636379, -2.144188719129172860 ) ) ;
#1811 = EDGE_CURVE ( 'NONE', #2201, #11805, #6261, .T. ) ;
#1812 = CARTESIAN_POINT ( 'NONE',  ( -20.63991140007999903, -5.133906642417999322, -9.805448442688000199 ) ) ;
#1813 = VERTEX_POINT ( 'NONE', #8483 ) ;
#1814 = VECTOR ( 'NONE', #7381, 1000.000000000000000 ) ;
#1815 = CARTESIAN_POINT ( 'NONE',  ( 1.549127279887130060, 23.82637683446857579, 1.758539927998388652 ) ) ;
#1816 = ORIENTED_EDGE ( 'NONE', *, *, #14709, .T. ) ;
#1817 = CARTESIAN_POINT ( 'NONE',  ( 2.291555368458999986, 24.21992044851000259, 0.5351892104662999694 ) ) ;
#1818 = CARTESIAN_POINT ( 'NONE',  ( 4.822430994633001511, 14.15577629170999430, 4.015704910791001225 ) ) ;
#1819 = CARTESIAN_POINT ( 'NONE',  ( 4.267029504470329471, 13.41085527056981697, 5.337432762833688393 ) ) ;
#1820 = B_SPLINE_CURVE_WITH_KNOTS ( 'NONE', 3,
 ( #17083, #9466, #481, #5593, #11408, #12975, #18669, #13095, #245, #9581, #366, #21081, #21451, #22886, #727, #4372, #11763, #21330, #17828, #23251, #15862, #4866, #13808, #6550, #6665, #15499, #10188, #19393, #8372, #17454, #4493, #13686, #4745, #12254, #15617, #6183, #23006, #13934, #10069, #12130, #1222, #19518 ),
 .UNSPECIFIED., .F., .F.,
 ( 4, 2, 1, 2, 2, 2, 1, 2, 2, 2, 2, 2, 2, 2, 2, 1, 2, 2, 2, 1, 2, 2, 4 ),
 ( 0.000000000000000000, 0.06250000000000002776, 0.09375000000000012490, 0.1093750000000000555, 0.1249999999999999722, 0.1874999999999998890, 0.2187499999999998335, 0.2343749999999998057, 0.2499999999999997502, 0.3124999999999997224, 0.3749999999999997780, 0.4999999999999996669, 0.5624999999999997780, 0.6249999999999998890, 0.6875000000000001110, 0.7187500000000004441, 0.7343750000000007772, 0.7500000000000011102, 0.8125000000000013323, 0.8437500000000013323, 0.8593750000000013323, 0.8750000000000014433, 1.000000000000000000 ),
 .UNSPECIFIED. ) ;
#1821 = CARTESIAN_POINT ( 'NONE',  ( 0.000000000000000000, 0.000000000000000000, 0.000000000000000000 ) ) ;
#1822 = PLANE ( 'NONE',  #14581 ) ;
#1823 = CARTESIAN_POINT ( 'NONE',  ( 11.77425158531000093, -9.807789133420998340, 1.022826625653000088 ) ) ;
#1824 = ORIENTED_EDGE ( 'NONE', *, *, #23121, .T. ) ;
#1825 = CARTESIAN_POINT ( 'NONE',  ( 0.000000000000000000, 24.65000000674550051, 0.000000000000000000 ) ) ;
#1826 = DIRECTION ( 'NONE',  ( -1.000000000000000000, 0.000000000000000000, 0.000000000000000000 ) ) ;
#1827 = DIRECTION ( 'NONE',  ( 1.000000000000000000, 0.000000000000000000, 0.000000000000000000 ) ) ;
#1828 = EDGE_CURVE ( 'NONE', #11598, #17995, #15849, .T. ) ;
#1829 = ORIENTED_EDGE ( 'NONE', *, *, #143, .F. ) ;
#1830 = CARTESIAN_POINT ( 'NONE',  ( -10.24525051287397304, 15.78812810035701908, -1.147541437844174839 ) ) ;
#1831 = AXIS2_PLACEMENT_3D ( 'NONE', #4906, #22804, #2722 ) ;
#1832 = CARTESIAN_POINT ( 'NONE',  ( 1.141652241544000024, 24.92002125539000090, -2.036977516418999823 ) ) ;
#1833 = CARTESIAN_POINT ( 'NONE',  ( 14.42230551843989339, -1.412630712418221357, -10.22074767084959213 ) ) ;
#1834 = CARTESIAN_POINT ( 'NONE',  ( -18.02909587121333956, 4.600144771116639220, -7.981067224362968560 ) ) ;
#1835 = CARTESIAN_POINT ( 'NONE',  ( 24.72504754407999883, -9.523234606517998913, 5.134017250187000059 ) ) ;
#1836 = CARTESIAN_POINT ( 'NONE',  ( 1.463521000971000019, 28.89991794178999740, -1.852106567100999968 ) ) ;
#1837 = CARTESIAN_POINT ( 'NONE',  ( 14.10065998436765611, 4.544368654919230366, 7.805219334371307660 ) ) ;
#1838 = CARTESIAN_POINT ( 'NONE',  ( 0.000000000000000000, 31.00000000000000000, 0.000000000000000000 ) ) ;
#1839 = CARTESIAN_POINT ( 'NONE',  ( -2.434931691670788378, 26.66753006952334104, 0.6543697108982053923 ) ) ;
#1840 = PLANE ( 'NONE',  #16418 ) ;
#1841 = EDGE_CURVE ( 'NONE', #10857, #7090, #3, .T. ) ;
#1842 = VERTEX_POINT ( 'NONE', #12240 ) ;
#1843 = CARTESIAN_POINT ( 'NONE',  ( 24.49999999999998934, -10.18003712748733314, 1.238246424670434775 ) ) ;
#1844 = AXIS2_PLACEMENT_3D ( 'NONE', #8315, #915, #4318 ) ;
#1845 = ORIENTED_EDGE ( 'NONE', *, *, #17835, .F. ) ;
#1846 = CARTESIAN_POINT ( 'NONE',  ( -15.80528743917331269, 7.258566966576419865, -5.578074939302383406 ) ) ;
#1847 = CARTESIAN_POINT ( 'NONE',  ( -7.500000000000000000, 18.50000000000000000, -2.000000000000000000 ) ) ;
#1848 = PLANE ( 'NONE',  #18900 ) ;
#1849 = CARTESIAN_POINT ( 'NONE',  ( 18.95627483587000128, 0.6520233587864000535, 11.11807124853999973 ) ) ;
#1850 = CARTESIAN_POINT ( 'NONE',  ( 0.000000000000000000, 24.00000000000000000, 0.000000000000000000 ) ) ;
#1851 = CARTESIAN_POINT ( 'NONE',  ( 1.996953125041000199, 26.30506359724000021, 1.450871306011999984 ) ) ;
#1852 = ORIENTED_EDGE ( 'NONE', *, *, #4997, .F. ) ;
#1853 = CARTESIAN_POINT ( 'NONE',  ( -11.22545756585000021, -11.56411535172999905, 9.345002482406000510 ) ) ;
#1854 = DIRECTION ( 'NONE',  ( 0.000000000000000000, -0.7071067811866525998, -0.7071067811864425456 ) ) ;
#1855 = CARTESIAN_POINT ( 'NONE',  ( 0.000000000000000000, 15.09999999999999964, -4.750000000000305533 ) ) ;
#1856 = EDGE_CURVE ( 'NONE', #13583, #3987, #13535, .T. ) ;
#1857 = VERTEX_POINT ( 'NONE', #18175 ) ;
#1858 = ADVANCED_FACE ( 'NONE', ( #3734 ), #3279, .T. ) ;
#1859 = DIRECTION ( 'NONE',  ( -1.000000000000000000, 0.000000000000000000, 0.000000000000000000 ) ) ;
#1860 = CARTESIAN_POINT ( 'NONE',  ( 19.97025975534796771, 8.314106973087666219, -6.433823374046138355 ) ) ;
#1861 = DIRECTION ( 'NONE',  ( 0.000000000000000000, -1.000000000000000000, 0.000000000000000000 ) ) ;
#1862 = CARTESIAN_POINT ( 'NONE',  ( 15.98099710151175756, -8.853047632443667325, -5.378228472014759731 ) ) ;
#1863 = CIRCLE ( 'NONE', #19664, 4.750000000000000000 ) ;
#1864 = CARTESIAN_POINT ( 'NONE',  ( -19.64339236541000133, -7.798846739588999100, 6.943248922331999751 ) ) ;
#1865 = CARTESIAN_POINT ( 'NONE',  ( -0.7569538692457000728, 28.77010822455999772, 2.088667364863999953 ) ) ;
#1866 = B_SPLINE_CURVE_WITH_KNOTS ( 'NONE', 3,
 ( #19014, #11761, #6419, #17200, #13805, #20718, #6052, #13441, #21202, #18776, #16964, #20844 ),
 .UNSPECIFIED., .F., .F.,
 ( 4, 1, 1, 1, 1, 2, 2, 4 ),
 ( 0.000000000000000000, 0.2500000000000006106, 0.3750000000000012768, 0.4375000000000013323, 0.4687500000000012768, 0.4843750000000014433, 0.5000000000000016653, 1.000000000000000000 ),
 .UNSPECIFIED. ) ;
#1867 = CARTESIAN_POINT ( 'NONE',  ( -15.35172225070999907, -1.839441420978000119, 9.553397381538999866 ) ) ;
#1868 = AXIS2_PLACEMENT_3D ( 'NONE', #9397, #17932, #6901 ) ;
#1869 = CARTESIAN_POINT ( 'NONE',  ( 1.939861484286318882, 29.86184696477200262, -0.9499241564717313402 ) ) ;
#1870 = EDGE_CURVE ( 'NONE', #5391, #16168, #3123, .T. ) ;
#1871 = ORIENTED_EDGE ( 'NONE', *, *, #18001, .T. ) ;
#1872 = CARTESIAN_POINT ( 'NONE',  ( 2.137452445837000337, 25.56179681940000137, 0.4573846582827000296 ) ) ;
#1873 = EDGE_CURVE ( 'NONE', #629, #3985, #10896, .T. ) ;
#1874 = CARTESIAN_POINT ( 'NONE',  ( 19.70340807481104406, -6.760929761475917843, -8.039421042557430397 ) ) ;
#1875 = CARTESIAN_POINT ( 'NONE',  ( -0.8818583641180756105, 23.65266154262563703, -1.963742263792713549 ) ) ;
#1876 = MECHANICAL_DESIGN_GEOMETRIC_PRESENTATION_REPRESENTATION (  '', ( #8060 ), #12344 ) ;
#1877 = VERTEX_POINT ( 'NONE', #8849 ) ;
#1878 = CARTESIAN_POINT ( 'NONE',  ( -6.370760730814999384, 15.09911243606998177, 3.226444468181998815 ) ) ;
#1879 = AXIS2_PLACEMENT_3D ( 'NONE', #18294, #3634, #18062 ) ;
#1880 = CARTESIAN_POINT ( 'NONE',  ( 4.833494560126003314, 12.42175294347999071, 0.1521608003744000515 ) ) ;
#1881 = CARTESIAN_POINT ( 'NONE',  ( 12.81825125731000092, -4.388733341911000174, 7.983506680731000671 ) ) ;
#1882 = ORIENTED_EDGE ( 'NONE', *, *, #15760, .T. ) ;
#1883 = DIRECTION ( 'NONE',  ( 0.000000000000000000, -1.000000000000000000, 0.000000000000000000 ) ) ;
#1884 = APPLICATION_PROTOCOL_DEFINITION ( 'draft international standard', 'automotive_design', 1998, #9733 ) ;
#1885 = FACE_OUTER_BOUND ( 'NONE', #18910, .T. ) ;
#1886 = VECTOR ( 'NONE', #18982, 1000.000000000000000 ) ;
#1887 = ORIENTED_EDGE ( 'NONE', *, *, #2096, .F. ) ;
#1888 = CARTESIAN_POINT ( 'NONE',  ( 22.32487270046334160, -9.003629214848199780, -2.419527782799394178 ) ) ;
#1889 = AXIS2_PLACEMENT_3D ( 'NONE', #5901, #22611, #9901 ) ;
#1890 = PRESENTATION_LAYER_ASSIGNMENT (  '', '', ( #23553 ) ) ;
#1891 = CARTESIAN_POINT ( 'NONE',  ( 11.99999999999999822, -1.778133311928435933, -9.288411946047254730 ) ) ;
#1892 = CARTESIAN_POINT ( 'NONE',  ( 11.59051697471232600, -8.994977951464667498, -9.420063436902960774 ) ) ;
#1893 = DIRECTION ( 'NONE',  ( 0.000000000000000000, -0.9998843904358519774, -0.01520545174352925036 ) ) ;
#1894 = CARTESIAN_POINT ( 'NONE',  ( -24.39605500772391622, 1.877234304591530289, -10.43857512010684196 ) ) ;
#1895 = CARTESIAN_POINT ( 'NONE',  ( 1.421749254172319565, 26.44307886155625198, -1.887007990465741081 ) ) ;
#1896 = DIRECTION ( 'NONE',  ( -0.000000000000000000, 1.000000000000000000, -0.000000000000000000 ) ) ;
#1897 = CARTESIAN_POINT ( 'NONE',  ( -6.382298667867003950, 15.08199981258001010, 3.360745759041997793 ) ) ;
#1898 = CARTESIAN_POINT ( 'NONE',  ( 1.635367627583443229, 30.69443307109471419, -1.412121873945937356 ) ) ;
#1899 = ORIENTED_EDGE ( 'NONE', *, *, #13827, .F. ) ;
#1900 = CARTESIAN_POINT ( 'NONE',  ( 0.000000000000000000, 8.900000000000000355, 0.000000000000000000 ) ) ;
#1901 = CARTESIAN_POINT ( 'NONE',  ( 14.68234440374828331, -4.311926369740707976, 8.013692814287820099 ) ) ;
#1902 = AXIS2_PLACEMENT_3D ( 'NONE', #23294, #14101, #21495 ) ;
#1903 = CARTESIAN_POINT ( 'NONE',  ( -21.17980191599842854, -9.824981607888839008, 3.766868870501678401 ) ) ;
#1904 = CARTESIAN_POINT ( 'NONE',  ( -1.739667959131000030, 26.94271896305999903, -1.485816803342000281 ) ) ;
#1905 = VECTOR ( 'NONE', #20072, 1000.000000000000000 ) ;
#1906 = CARTESIAN_POINT ( 'NONE',  ( 3.689409531404894249, 12.05188896767502627, 3.123460345082171408 ) ) ;
#1907 = ORIENTED_EDGE ( 'NONE', *, *, #81, .T. ) ;
#1908 = CARTESIAN_POINT ( 'NONE',  ( -1.842032823788972928, 11.62708128007210817, -4.451304217208804204 ) ) ;
#1909 = CARTESIAN_POINT ( 'NONE',  ( 24.31126325372243357, 8.589904588849305966, -4.641259051888694920 ) ) ;
#1910 = AXIS2_PLACEMENT_3D ( 'NONE', #21327, #16229, #10553 ) ;
#1911 = CARTESIAN_POINT ( 'NONE',  ( 0.000000000000000000, 24.29999999999999716, 0.000000000000000000 ) ) ;
#1912 = VERTEX_POINT ( 'NONE', #18048 ) ;
#1913 = CARTESIAN_POINT ( 'NONE',  ( -23.76320766698999876, 13.93375672974000068, 0.0006662677302622000038 ) ) ;
#1914 = CARTESIAN_POINT ( 'NONE',  ( 13.96800158531000058, -3.572926710108999870, -9.509691282521000488 ) ) ;
#1915 = CARTESIAN_POINT ( 'NONE',  ( 18.28194284694450644, 6.412433293717898941, -8.218262321110563207 ) ) ;
#1916 = AXIS2_PLACEMENT_3D ( 'NONE', #16614, #22, #8137 ) ;
#1917 = DIRECTION ( 'NONE',  ( -1.000000000000000000, 0.000000000000000000, 0.000000000000000000 ) ) ;
#1918 = CARTESIAN_POINT ( 'NONE',  ( -2.017184895920000276, 29.29859001081999992, -0.7461322788111000026 ) ) ;
#1919 = CARTESIAN_POINT ( 'NONE',  ( 19.11921080085999947, -6.083244085703999993, 8.615239357168999135 ) ) ;
#1920 = CARTESIAN_POINT ( 'NONE',  ( -24.50000000000000000, -1.873582633960999999, -10.39897383761999983 ) ) ;
#1921 = AXIS2_PLACEMENT_3D ( 'NONE', #17760, #13992, #14359 ) ;
#1922 = ORIENTED_EDGE ( 'NONE', *, *, #11094, .F. ) ;
#1923 = CARTESIAN_POINT ( 'NONE',  ( 0.000000000000000000, 15.00000000000000000, 0.000000000000000000 ) ) ;
#1924 = CARTESIAN_POINT ( 'NONE',  ( 22.34344591821000137, 10.66184160259999913, -1.641226805065000072 ) ) ;
#1925 = CARTESIAN_POINT ( 'NONE',  ( 0.000000000000000000, 22.00131761696259503, 0.000000000000000000 ) ) ;
#1926 = ORIENTED_EDGE ( 'NONE', *, *, #8029, .T. ) ;
#1927 = CARTESIAN_POINT ( 'NONE',  ( 24.50000000000000000, -5.768522138344023276, 8.866799569317205254 ) ) ;
#1928 = CARTESIAN_POINT ( 'NONE',  ( 6.124999911758999716, 14.37502625872000195, -0.0001546258496581000123 ) ) ;
#1929 = CARTESIAN_POINT ( 'NONE',  ( -3.235268519333999393, 11.88803707044000824, 3.615098393403000099 ) ) ;
#1930 = CARTESIAN_POINT ( 'NONE',  ( 0.2764502732170818211, 29.18736629261196214, -2.142238836452773576 ) ) ;
#1931 = DIRECTION ( 'NONE',  ( 0.000000000000000000, 0.000000000000000000, 1.000000000000000000 ) ) ;
#1932 = ORIENTED_EDGE ( 'NONE', *, *, #2874, .T. ) ;
#1933 = VERTEX_POINT ( 'NONE', #9308 ) ;
#1934 = EDGE_CURVE ( 'NONE', #15539, #15097, #1560, .T. ) ;
#1935 = CARTESIAN_POINT ( 'NONE',  ( 2.349836359248000051, 25.05596380282000268, -0.1261848867558000020 ) ) ;
#1936 = CARTESIAN_POINT ( 'NONE',  ( 5.081323529022999885, 13.95840221409999771, 4.282381695897004015 ) ) ;
#1937 = CARTESIAN_POINT ( 'NONE',  ( 16.42937270046333254, -2.379927906264107662, 8.856276743063176582 ) ) ;
#1938 = LINE ( 'NONE', #224, #1814 ) ;
#1939 = DIRECTION ( 'NONE',  ( 0.000000000000000000, 1.000000000000000000, 0.000000000000000000 ) ) ;
#1940 = CARTESIAN_POINT ( 'NONE',  ( 14.84550158531000008, 4.534570621724000716, 9.116298118718001220 ) ) ;
#1941 = B_SPLINE_CURVE_WITH_KNOTS ( 'NONE', 3,
 ( #9921, #21061, #13916, #4971, #4725, #11991, #19117, #4474, #11863, #6531, #21312, #12113, #19499, #2908, #10290, #1078, #23232, #6645, #4847, #21906, #14284, #12707, #8957, #9184, #3510, #23951, #19857, #21791, #14743, #19745, #16325, #9066, #6891, #5438, #16081, #14399, #16209, #16561, #12588, #8844, #7358, #21679, #5206, #18170, #19975, #7122, #14512, #7237, #16437, #10655, #11000, #12471, #14628, #10891, #3272, #1676, #22136, #18277, #3394, #5091, #22025, #3155, #12819, #20212, #3617, #8717, #1448, #17923, #12356, #10538, #23606, #18385, #7011, #23828, #10778, #23716, #1328, #1573, #1796, #23480, #5317, #18043, #20099, #19320, #86, #6228, #6350, #14855, #3853, #7470, #17501, #18624, #20894, #22932, #894, #17252, #11246, #13733, #529, #5660, #8177, #21130, #776, #20441, #15300, #15545, #8297, #15426, #11119, #4300, #18505, #1915, #3730, #4541, #8053, #22812, #16678, #9304, #19188, #11934, #2031, #9421, #16791, #2729, #10111, #15661, #5547, #7933, #22691, #22243, #12925, #651, #9989, #6101, #13494, #20322, #11690, #13045, #19064, #2478, #9867, #13610, #21008, #4420, #11811, #2597, #17377, #3341, #17625, #5155, #12536, #18110, #14103, #4672, #19923, #23548, #12298, #1517, #19686, #6710, #8658, #1019, #23417, #3102, #10718, #14227, #8907, #6598, #8548, #23051, #6473, #10487, #19808, #8421, #16146, #2851, #1154, #2970, #13857, #23297, #19566, #12056, #15789, #15905, #4910, #21498, #17873, #1272, #17990, #3223, #21374, #21741, #23181, #1392, #21623, #13982, #12424, #21261, #5042, #16022, #4790, #19442, #10232, #8784, #6959, #14350, #12175, #10360, #17749, #6835, #10605, #5382, #11193, #10951, #12993, #14694, #20275, #5266, #22086, #5730, #13117, #12652, #3679, #9251, #12770, #23779, #14460, #1628, #21968, #7186, #7303, #9018, #3458, #14920, #16387, #20515, #3920, #21855, #11070, #11312, #1746, #18576, #20394, #18453, #16628, #10843, #7076, #5495, #16508, #20040, #12875, #1862, #18227, #9133, #14575, #20160, #3567, #18337, #23896, #38, #7420, #14803, #18688, #148, #9364, #2094, #16273, #22198, #5611, #1981, #23665, #3799, #16738, #7540, #22314, #17344, #13706, #16861, #19158, #11783, #748, #7787, #2568, #20982, #19287, #2448, #8152, #505, #9959, #16989, #21099, #13586, #4034, #20624, #15274, #263, #22438, #13465, #9841, #5958, #390, #17222, #15517, #18802, #15157, #11428, #4513, #22552, #7905, #22905, #11904, #20868, #13343, #6321, #4150, #9602, #9484, #4392, #4278, #621, #6074, #7668, #15042, #19038, #5848, #22665, #13231, #2211, #20742, #11546, #11666, #8023, #18926, #2335, #22785, #9724, #15395, #6201, #17106, #21347, #12148, #15993, #6569, #19781, #17721, #1118, #1363, #6442, #23148, #23268, #8393, #23025, #3191, #4641, #10573, #17846, #12508, #17472, #21596, #8520, #15634, #8630, #10204, #1239, #8270, #5125, #23386, #13953, #10457, #14074, #2701, #19658, #17959, #15878, #12397, #17597, #14327, #6805, #21228, #13830, #6682, #12029, #21469, #3072, #4762, #991, #866, #19410, #15758, #19536, #4882, #2824, #2942, #8752, #10331, #23519, #6930, #12271, #14199, #21715, #5011, #16118, #10085, #7273, #20247, #16475, #10815, #16363, #12964, #1951, #14891, #22171, #1607, #5351, #7049, #16709, #14665, #9, #18206, #12740, #22282, #10925, #11039, #8992, #14546, #20134, #10690, #1486, #22060, #3769, #5469, #21941, #121, #14432, #9337, #7508, #5697, #18312, #8880, #19893, #20360, #3309, #18080, #14775, #1713, #16250, #21827, #3653, #23866, #23643, #18422, #5240, #3431, #3542, #12625, #20010, #12851, #16598, #23752, #11157, #7156, #1833, #9103, #9219, #7392, #5582, #18543, #22408, #15123, #18892, #20709, #7871, #15239, #7990, #9806, #11397, #11750, #13199, #15362, #11636, #4001, #16829, #7636, #4358, #16955, #20953, #17312, #20482, #22753, #6172, #19122, #9455, #2177, #18658, #2064, #4118, #233, #15010, #11281, #13555, #22632, #17189, #18767, #22518, #15487, #11516, #5817, #2535, #2303, #9689, #9570, #2415, #355, #9927, #17070, #468, #714, #20592, #7755, #6043, #5927, #13432, #13311, #8123, #22873, #20833 ),
 .UNSPECIFIED., .F., .F.,
 ( 4, 2, 2, 2, 1, 1, 2, 2, 1, 1, 2, 2, 2, 1, 2, 2, 1, 2, 2, 2, 2, 2, 1, 1, 1, 1, 1, 2, 2, 2, 2, 2, 1, 1, 2, 2, 1, 1, 2, 2, 2, 2, 2, 2, 1, 1, 2, 2, 1, 2, 2, 2, 2, 1, 1, 2, 2, 2, 2, 2, 2, 2, 1, 1, 1, 2, 2, 2, 2, 2, 2, 2, 2, 1, 2, 2, 1, 1, 2, 2, 2, 2, 1, 1, 1, 1, 1, 1, 1, 1, 2, 2, 2, 2, 2, 2, 2, 2, 2, 2, 2, 2, 2, 2, 2, 2, 2, 2, 2, 2, 2, 2, 2, 2, 2, 1, 1, 1, 1, 1, 1, 2, 2, 2, 2, 1, 1, 1, 1, 1, 2, 2, 2, 2, 2, 1, 1, 1, 1, 1, 2, 2, 2, 2, 2, 1, 1, 1, 1, 2, 2, 2, 2, 1, 1, 1, 2, 2, 2, 2, 2, 1, 2, 2, 2, 2, 1, 1, 2, 2, 2, 2, 2, 2, 2, 1, 1, 1, 1, 1, 2, 2, 2, 2, 2, 1, 1, 1, 2, 2, 2, 2, 1, 1, 1, 1, 1, 2, 2, 2, 2, 2, 2, 2, 2, 2, 1, 1, 1, 1, 1, 2, 2, 2, 2, 2, 1, 1, 1, 1, 1, 2, 2, 2, 2, 2, 1, 1, 1, 2, 2, 2, 2, 1, 1, 1, 1, 1, 1, 2, 2, 2, 2, 2, 1, 1, 1, 1, 1, 2, 2, 2, 2, 2, 1, 1, 2, 2, 1, 1, 2, 2, 2, 2, 2, 2, 2, 2, 2, 2, 1, 1, 1, 1, 1, 2, 2, 2, 2, 2, 2, 1, 2, 2, 1, 1, 1, 2, 2, 2, 2, 2, 2, 2, 1, 1, 1, 1, 2, 2, 2, 2, 2, 2, 2, 2, 2, 2, 2, 1, 1, 1, 1, 2, 2, 2, 2, 2, 2, 2, 2, 4 ),
 ( 0.000000000000000000, 0.007812499999996756067, 0.01562499999999351213, 0.01953124999999188843, 0.02050781249999149639, 0.02075195312499140618, 0.02081298828124138883, 0.02087402343749137149, 0.02099609374999134720, 0.02148437499999125699, 0.02343749999999087535, 0.03124999999998935574, 0.03906249999998783612, 0.04101562499998746142, 0.04150390624998735734, 0.04174804687498730876, 0.04199218749998725325, 0.04296874999998700345, 0.04687499999998599731, 0.05468749999998395034, 0.05859374999998293726, 0.06054687499998243072, 0.06152343749998217398, 0.06201171874998204214, 0.06225585937498197969, 0.06237792968748194500, 0.06243896484373193806, 0.06246948242185692418, 0.06249999999998190336, 0.07031249999997722655, 0.07812499999997254974, 0.08203124999997023215, 0.08300781249996963540, 0.08325195312496949662, 0.08331298828121945499, 0.08337402343746941336, 0.08349609374996934397, 0.08398437499996899702, 0.08593749999996766475, 0.09374999999996232181, 0.09570312499996098954, 0.09765624999995964339, 0.1015624999999569789, 0.1054687499999543143, 0.1064453124999536482, 0.1069335937499533151, 0.1070556640624532319, 0.1071777343749531486, 0.1074218749999530514, 0.1093749999999521771, 0.1132812499999504147, 0.1171874999999486522, 0.1181640624999482220, 0.1186523437499479999, 0.1188964843749478889, 0.1190185546874478195, 0.1191406249999477501, 0.1210937499999469313, 0.1249999999999452799, 0.1289062499999436562, 0.1308593749999428235, 0.1309814453124427958, 0.1311035156249427402, 0.1313476562499426015, 0.1318359374999423239, 0.1328124999999417688, 0.1406249999999372169, 0.1484374999999326650, 0.1562499999999281408, 0.1640624999999235889, 0.1718749999999190370, 0.1757812499999167610, 0.1777343749999156231, 0.1782226562499153455, 0.1784667968749151790, 0.1785888671874150957, 0.1787109374999150124, 0.1796874999999144296, 0.1874999999999097111, 0.2031249999999002742, 0.2187499999998908651, 0.2343749999998814282, 0.2421874999998767097, 0.2460937499998743505, 0.2480468749998731848, 0.2490234374998726019, 0.2495117187498722966, 0.2497558593748721578, 0.2498779296873720746, 0.2499389648436220468, 0.2499694824217470190, 0.2499999999998720190, 0.2578124999998676059, 0.2656249999998631095, 0.2734374999998586686, 0.2812499999998541722, 0.2890624999998497313, 0.2968749999998452349, 0.3046874999998407940, 0.3124999999998363531, 0.3203124999998318567, 0.3281249999998274158, 0.3437499999998185340, 0.3515624999998140376, 0.3593749999998096523, 0.3749999999998007705, 0.3906249999997918887, 0.4062499999997830069, 0.4218749999997741251, 0.4374999999997652989, 0.4531249999997564171, 0.4687499999997475353, 0.4843749999997386535, 0.4921874999997341571, 0.4960937499997319367, 0.4980468749997308819, 0.4990234374997302713, 0.4995117187497300493, 0.4997558593747298827, 0.4998779296872298272, 0.4999389648434798272, 0.4999694824216048827, 0.4999999999997299382, 0.5078124999997339906, 0.5117187499997359890, 0.5136718749997369882, 0.5146484374997374323, 0.5151367187497376543, 0.5153808593747377653, 0.5155029296872378763, 0.5155639648434878763, 0.5156249999997378763, 0.5234374999997412070, 0.5273437499997429834, 0.5292968749997437605, 0.5302734374997442046, 0.5307617187497444267, 0.5310058593747445377, 0.5311279296872446487, 0.5311889648434945377, 0.5312194824216195377, 0.5312499999997445377, 0.5390624999997504219, 0.5429687499997533084, 0.5449218749997548628, 0.5458984374997555289, 0.5463867187497559730, 0.5466308593747561950, 0.5467529296872561950, 0.5468139648435063060, 0.5468749999997564171, 0.5507812499997595257, 0.5527343749997611910, 0.5537109374997619682, 0.5541992187497623013, 0.5544433593747625233, 0.5545654296872626343, 0.5546874999997626343, 0.5585937499997662981, 0.5605468749997680744, 0.5615234374997689626, 0.5620117187497694067, 0.5622558593747696287, 0.5624999999997698508, 0.5664062499997735145, 0.5683593749997752909, 0.5693359374997762901, 0.5698242187497767341, 0.5700683593747769562, 0.5703124999997771782, 0.5742187499997807310, 0.5781249999997843947, 0.5859374999997915001, 0.5898437499997950528, 0.5917968749997968292, 0.5927734374997977174, 0.5932617187497981615, 0.5935058593747983835, 0.5936279296872984945, 0.5936889648435486055, 0.5937194824216734945, 0.5937499999997984945, 0.6015624999998055999, 0.6054687499998091527, 0.6074218749998108180, 0.6083984374998118172, 0.6088867187498122613, 0.6091308593748124833, 0.6092529296873124833, 0.6093749999998125944, 0.6171874999998200328, 0.6210937499998236966, 0.6230468749998255840, 0.6240234374998264721, 0.6245117187498269162, 0.6247558593748271383, 0.6248779296873273603, 0.6249389648435774713, 0.6249999999998274713, 0.6406249999998402389, 0.6562499999998530065, 0.6640624999998593347, 0.6718749999998657740, 0.6796874999998722133, 0.6835937499998753220, 0.6855468749998769873, 0.6865234374998777644, 0.6870117187498782085, 0.6872558593748784306, 0.6873779296873784306, 0.6874389648436285416, 0.6874694824217535416, 0.6874999999998785416, 0.6953124999998835376, 0.6992187499998859801, 0.7011718749998873124, 0.7021484374998878675, 0.7026367187498882005, 0.7028808593748883116, 0.7030029296873884226, 0.7030639648436385336, 0.7030944824217634226, 0.7031249999998884226, 0.7109374999998898659, 0.7148437499998905320, 0.7167968749998908651, 0.7177734374998910871, 0.7182617187498911981, 0.7185058593748911981, 0.7186279296873911981, 0.7187499999998913092, 0.7265624999998921973, 0.7304687499998925304, 0.7324218749998927525, 0.7333984374998928635, 0.7338867187498928635, 0.7341308593748928635, 0.7342529296873929745, 0.7343139648436429745, 0.7343444824217679745, 0.7343749999998928635, 0.7421874999998934186, 0.7460937499998937517, 0.7480468749998938627, 0.7490234374998939737, 0.7495117187498939737, 0.7497558593748939737, 0.7498779296873939737, 0.7499389648436439737, 0.7499694824217689737, 0.7499999999998939737, 0.7578124999998957501, 0.7656249999998975264, 0.7695312499998984146, 0.7705078124998986366, 0.7707519531248986366, 0.7708129882811486366, 0.7708740234373986366, 0.7709960937498986366, 0.7714843749998987477, 0.7734374999998988587, 0.7812499999998996358, 0.7890624999999004130, 0.7910156249999006350, 0.7919921874999006350, 0.7929687499999006350, 0.7968749999999010791, 0.8046874999999016342, 0.8085937499999020783, 0.8105468749999023004, 0.8115234374999023004, 0.8120117187499023004, 0.8122558593749023004, 0.8123779296874023004, 0.8124389648436521894, 0.8124694824217771894, 0.8124999999999021894, 0.8203124999999076294, 0.8281249999999130695, 0.8320312499999157341, 0.8330078124999165112, 0.8332519531249166223, 0.8333129882811666223, 0.8333435058592916223, 0.8333740234374166223, 0.8334960937499167333, 0.8339843749999170663, 0.8359374999999186207, 0.8437499999999246159, 0.8515624999999307221, 0.8593749999999368283, 0.8671874999999429345, 0.8710937499999459321, 0.8730468749999474865, 0.8740234374999481526, 0.8745117187499484857, 0.8747558593749487077, 0.8748779296874488187, 0.8749389648436989297, 0.8749999999999489297, 0.8828124999999543698, 0.8906249999999598099, 0.8984374999999652500, 0.9062499999999706901, 0.9140624999999760192, 0.9218749999999814593, 0.9296874999999868994, 0.9335937499999895639, 0.9355468749999910072, 0.9365234374999916733, 0.9370117187499921174, 0.9372558593749922284, 0.9373779296874923395, 0.9374389648437423395, 0.9374999999999923395, 0.9531249999999942268, 0.9609374999999952260, 0.9687499999999962252, 0.9765624999999972244, 0.9843749999999981126, 0.9921874999999991118, 1.000000000000000000 ),
 .UNSPECIFIED. ) ;
#1942 = VERTEX_POINT ( 'NONE', #1920 ) ;
#1943 = CARTESIAN_POINT ( 'NONE',  ( -12.50789737913000010, 5.572872693153001045, -7.876595158781000805 ) ) ;
#1944 = AXIS2_PLACEMENT_3D ( 'NONE', #1453, #18509, #23612 ) ;
#1945 = CARTESIAN_POINT ( 'NONE',  ( 0.000000000000000000, 17.00000000000000000, 0.000000000000000000 ) ) ;
#1946 = CARTESIAN_POINT ( 'NONE',  ( 4.649999999999999467, 20.00000000000000000, 0.000000000000000000 ) ) ;
#1947 = ORIENTED_EDGE ( 'NONE', *, *, #9271, .T. ) ;
#1948 = EDGE_CURVE ( 'NONE', #16694, #16650, #11470, .T. ) ;
#1949 = CARTESIAN_POINT ( 'NONE',  ( -6.250000000000000000, 16.31160201366999729, -1.000000000001000089 ) ) ;
#1950 = CARTESIAN_POINT ( 'NONE',  ( -1.384310211871999874, 25.30426794178999828, 1.880513647577999992 ) ) ;
#1951 = CARTESIAN_POINT ( 'NONE',  ( 14.77879143498036285, 9.187885709464108430, -4.717911039109739413 ) ) ;
#1952 = CARTESIAN_POINT ( 'NONE',  ( -18.44480420454666714, -7.312553030913967689, -5.619880916868769560 ) ) ;
#1953 = CARTESIAN_POINT ( 'NONE',  ( 23.31785416133999789, -6.911498531077999274, -8.917763646754000462 ) ) ;
#1954 = CARTESIAN_POINT ( 'NONE',  ( 0.1485877089535999895, 30.08704325201000174, 2.548780468506000041 ) ) ;
#1955 = CARTESIAN_POINT ( 'NONE',  ( 13.69882080557875881, 8.479719668256132437, -3.078924866922988279 ) ) ;
#1956 = CARTESIAN_POINT ( 'NONE',  ( -4.810356821045001396, 12.64187851441000454, -0.3304506023919999147 ) ) ;
#1957 =( LENGTH_UNIT ( ) NAMED_UNIT ( * ) SI_UNIT ( .MILLI., .METRE. ) );
#1958 = CARTESIAN_POINT ( 'NONE',  ( 22.26465740196000098, 7.788096699281999769, 8.394476371801001591 ) ) ;
#1959 = ORIENTED_EDGE ( 'NONE', *, *, #8542, .F. ) ;
#1960 = CARTESIAN_POINT ( 'NONE',  ( -1.806240660677517873, 24.33331728578134090, 1.776608537230899509 ) ) ;
#1961 = CARTESIAN_POINT ( 'NONE',  ( 0.7318187998270078154, 29.87490599056237528, -4.196286372439439027 ) ) ;
#1962 = ORIENTED_EDGE ( 'NONE', *, *, #6661, .T. ) ;
#1963 = EDGE_CURVE ( 'NONE', #6244, #20885, #20141, .T. ) ;
#1964 = CARTESIAN_POINT ( 'NONE',  ( -16.48553743917331360, -9.094333095012673951, -1.190572366013357586 ) ) ;
#1965 = CARTESIAN_POINT ( 'NONE',  ( 24.18393254356834277, 8.381833107684220963, 10.48223919692640393 ) ) ;
#1966 = CARTESIAN_POINT ( 'NONE',  ( 22.17370603379667671, -8.999753784811684199, 2.418746970030813959 ) ) ;
#1967 = CARTESIAN_POINT ( 'NONE',  ( 15.52770777679999981, -6.525431417549000024, 8.909778109634999055 ) ) ;
#1968 = AXIS2_PLACEMENT_3D ( 'NONE', #17301, #700, #8109 ) ;
#1969 = FACE_OUTER_BOUND ( 'NONE', #5237, .T. ) ;
#1970 = CARTESIAN_POINT ( 'NONE',  ( 0.5485649090616000478, 28.50712896666999896, 2.437990915149000237 ) ) ;
#1971 = ORIENTED_EDGE ( 'NONE', *, *, #154, .T. ) ;
#1972 = ORIENTED_EDGE ( 'NONE', *, *, #2264, .T. ) ;
#1973 = CARTESIAN_POINT ( 'NONE',  ( -10.81079363876999899, 4.622502607133999852, -14.49941598755999905 ) ) ;
#1974 = CARTESIAN_POINT ( 'NONE',  ( 1.524598462963647538, 6.946544218151612604, -0.8912506324979003747 ) ) ;
#1975 = CARTESIAN_POINT ( 'NONE',  ( -14.49454820080683781, -11.34301321103862215, -5.353338751774003867 ) ) ;
#1976 = ORIENTED_EDGE ( 'NONE', *, *, #7285, .F. ) ;
#1977 = EDGE_CURVE ( 'NONE', #5360, #13125, #15211, .T. ) ;
#1978 = DIRECTION ( 'NONE',  ( 0.000000000000000000, 0.000000000000000000, -1.000000000000000000 ) ) ;
#1979 = CARTESIAN_POINT ( 'NONE',  ( 19.38196803061413576, -9.569877228560322635, -4.561946182171338293 ) ) ;
#1980 = CARTESIAN_POINT ( 'NONE',  ( 24.38510397947347386, 9.380175294669545139, -8.753059805729597187 ) ) ;
#1981 = CARTESIAN_POINT ( 'NONE',  ( 15.92416512556680352, -9.758728831869941445, -3.476723394276768797 ) ) ;
#1982 = CARTESIAN_POINT ( 'NONE',  ( -19.46272905036999745, -11.08280635929999924, 1.130260105365999967 ) ) ;
#1983 = CARTESIAN_POINT ( 'NONE',  ( -2.179000003682999953, 30.77442081890999859, -0.2443071251729000137 ) ) ;
#1984 = CARTESIAN_POINT ( 'NONE',  ( -16.65202050098999820, 5.360250747359000201, -9.417511137717001546 ) ) ;
#1985 = EDGE_CURVE ( 'NONE', #16663, #13308, #14974, .T. ) ;
#1986 = CARTESIAN_POINT ( 'NONE',  ( 0.7927445159862746005, 29.65171683346636300, 2.009466139971896492 ) ) ;
#1987 = ORIENTED_EDGE ( 'NONE', *, *, #12666, .T. ) ;
#1988 = CARTESIAN_POINT ( 'NONE',  ( -2.042880948895999804, 25.38708707564000022, -0.7651981593944000570 ) ) ;
#1989 = CARTESIAN_POINT ( 'NONE',  ( 20.69647650300873210, 4.117193616373135967, 9.695396857088221410 ) ) ;
#1990 = CARTESIAN_POINT ( 'NONE',  ( -18.22510727069612102, 4.477738147576441285, 9.453292167412891800 ) ) ;
#1991 = VERTEX_POINT ( 'NONE', #22724 ) ;
#1992 = EDGE_CURVE ( 'NONE', #8805, #1761, #374, .T. ) ;
#1993 = CARTESIAN_POINT ( 'NONE',  ( 12.50897733419000168, 7.466846271614999253, 11.77833069256000087 ) ) ;
#1994 = CARTESIAN_POINT ( 'NONE',  ( -5.310415759193001684, 14.71388207620999466, 3.630273082683998176 ) ) ;
#1995 = ADVANCED_FACE ( 'NONE', ( #2386 ), #3858, .F. ) ;
#1996 = DIRECTION ( 'NONE',  ( -1.000000000000000000, 0.000000000000000000, 0.000000000000000000 ) ) ;
#1997 = CARTESIAN_POINT ( 'NONE',  ( 17.67093892131000032, 6.655236401869999874, -7.121176743063999837 ) ) ;
#1998 = PRODUCT_DEFINITION_CONTEXT ( 'detailed design', #23802, 'design' ) ;
#1999 = ORIENTED_EDGE ( 'NONE', *, *, #12962, .T. ) ;
#2000 = DIRECTION ( 'NONE',  ( 0.000000000000000000, -1.000000000000000000, 0.000000000000000000 ) ) ;
#2001 = CARTESIAN_POINT ( 'NONE',  ( -14.39391695409897665, 4.126581034334551035, -12.49998949086425526 ) ) ;
#2002 = AXIS2_PLACEMENT_3D ( 'NONE', #526, #8174, #6225 ) ;
#2003 = ORIENTED_EDGE ( 'NONE', *, *, #2450, .F. ) ;
#2004 = EDGE_CURVE ( 'NONE', #4259, #21619, #1735, .T. ) ;
#2005 = CARTESIAN_POINT ( 'NONE',  ( 22.62720603379666073, -2.421793114379757750, -9.011088590333773851 ) ) ;
#2006 = CARTESIAN_POINT ( 'NONE',  ( -4.736789979881001145, 12.61336825782000481, -0.1514565667017998829 ) ) ;
#2007 = CARTESIAN_POINT ( 'NONE',  ( -21.65474665972999802, -2.779264633183000210, -9.192073190559000295 ) ) ;
#2008 = DIRECTION ( 'NONE',  ( 0.000000000000000000, 1.000000000000000000, 0.000000000000000000 ) ) ;
#2009 = FACE_OUTER_BOUND ( 'NONE', #12066, .T. ) ;
#2010 = CARTESIAN_POINT ( 'NONE',  ( -20.61299152281980085, 6.891406388424135443, -7.933605387358306338 ) ) ;
#2011 = CARTESIAN_POINT ( 'NONE',  ( 0.000000000000000000, 24.29999999999999716, -2.750000000000000000 ) ) ;
#2012 = LINE ( 'NONE', #23616, #6899 ) ;
#2013 = CARTESIAN_POINT ( 'NONE',  ( -6.002899204263999700, 16.48938829593000222, 1.302400215941999617 ) ) ;
#2014 = CARTESIAN_POINT ( 'NONE',  ( -0.6556536848882291713, 30.36463005559760120, 2.057991541314201367 ) ) ;
#2015 = ORIENTED_EDGE ( 'NONE', *, *, #17636, .T. ) ;
#2016 = CARTESIAN_POINT ( 'NONE',  ( 23.26647781200000153, 8.343268572584999987, 5.276840896087999333 ) ) ;
#2017 = CARTESIAN_POINT ( 'NONE',  ( 4.950289441944255131, 13.61399942321605927, -4.797373584915786360 ) ) ;
#2018 = CARTESIAN_POINT ( 'NONE',  ( -23.48257016776725337, 4.959647080842567668, 9.349265232667463010 ) ) ;
#2019 = CARTESIAN_POINT ( 'NONE',  ( 1.741868208726000011, 27.12196440326000157, 1.741868208726000011 ) ) ;
#2020 = CARTESIAN_POINT ( 'NONE',  ( -3.657438266360000245, 26.50000000000000000, 3.657438266360000245 ) ) ;
#2021 = AXIS2_PLACEMENT_3D ( 'NONE', #8540, #21962, #19802 ) ;
#2022 = DIRECTION ( 'NONE',  ( 0.000000000000000000, -1.000000000000000000, 0.000000000000000000 ) ) ;
#2023 = ORIENTED_EDGE ( 'NONE', *, *, #15286, .T. ) ;
#2024 = CARTESIAN_POINT ( 'NONE',  ( -3.348221499849736826, 11.95344782507623194, -3.481183559751760637 ) ) ;
#2025 = DIRECTION ( 'NONE',  ( 0.000000000000000000, 0.9512662730843030046, -0.3083706822840010520 ) ) ;
#2026 = CARTESIAN_POINT ( 'NONE',  ( -3.999878274658705823, 28.13336607547242352, 1.519686587934141242 ) ) ;
#2027 = ORIENTED_EDGE ( 'NONE', *, *, #9911, .F. ) ;
#2028 = EDGE_CURVE ( 'NONE', #3203, #18824, #5426, .T. ) ;
#2029 = CARTESIAN_POINT ( 'NONE',  ( 24.00034722001000276, -6.716786536054000223, 12.21137788280000080 ) ) ;
#2030 = CARTESIAN_POINT ( 'NONE',  ( 17.14893908531000122, -9.665900270332999256, 3.387665420544000217 ) ) ;
#2031 = CARTESIAN_POINT ( 'NONE',  ( 18.07779827556542074, -0.4281578631263728285, -10.40548960717138272 ) ) ;
#2032 = CARTESIAN_POINT ( 'NONE',  ( -24.47970833437514315, 1.023963593981846776, 12.49997010189808044 ) ) ;
#2033 = CARTESIAN_POINT ( 'NONE',  ( 0.3592561569125999887, 29.66874352329000075, 2.314061945504000128 ) ) ;
#2034 = CARTESIAN_POINT ( 'NONE',  ( 13.63483580085999947, -5.096719188837999681, 10.08552589914000031 ) ) ;
#2035 = CARTESIAN_POINT ( 'NONE',  ( -1.767114192125461614, 30.87940659144713962, -1.172702609216230485 ) ) ;
#2036 = AXIS2_PLACEMENT_3D ( 'NONE', #3244, #1859, #13886 ) ;
#2037 = VERTEX_POINT ( 'NONE', #203 ) ;
#2038 = DIRECTION ( 'NONE',  ( 0.000000000000000000, -1.000000000000000000, 0.000000000000000000 ) ) ;
#2039 = CARTESIAN_POINT ( 'NONE',  ( 20.57295489666000066, 10.73902819488999860, -0.02183603347782999901 ) ) ;
#2040 = CARTESIAN_POINT ( 'NONE',  ( -24.12340887139987089, 7.182491261854132780, 6.898148839887506156 ) ) ;
#2041 = EDGE_LOOP ( 'NONE', ( #19969, #19071, #19671, #2961 ) ) ;
#2042 = CARTESIAN_POINT ( 'NONE',  ( 12.26599830533000102, 1.737683063983999965, -9.170090943151999241 ) ) ;
#2043 = LINE ( 'NONE', #3742, #15291 ) ;
#2044 = CARTESIAN_POINT ( 'NONE',  ( -4.821039626244001397, 12.41688405863999378, 0.4163202411090001220 ) ) ;
#2045 = CARTESIAN_POINT ( 'NONE',  ( 1.962415512518493221, 29.05860578903570968, -0.9022275906645381705 ) ) ;
#2046 = CARTESIAN_POINT ( 'NONE',  ( -23.14617958678999798, -2.878374533911999933, 10.75773347001999802 ) ) ;
#2047 = VERTEX_POINT ( 'NONE', #9661 ) ;
#2048 = CARTESIAN_POINT ( 'NONE',  ( -1.671768471690028512, 23.69914749046346003, 1.453238603757796232 ) ) ;
#2049 = ORIENTED_EDGE ( 'NONE', *, *, #9059, .F. ) ;
#2050 = CARTESIAN_POINT ( 'NONE',  ( 1.526497572355999921, 24.35926100756000068, -1.790937938634000082 ) ) ;
#2051 = CARTESIAN_POINT ( 'NONE',  ( 1.259047450927256895, 28.26666666666667282, 2.184465970885639763 ) ) ;
#2052 = CARTESIAN_POINT ( 'NONE',  ( -1.184521108792000010, 28.36049822781000174, -1.932944458086000017 ) ) ;
#2053 = CARTESIAN_POINT ( 'NONE',  ( 0.000000000000000000, -1.100000000000000089, 0.000000000000000000 ) ) ;
#2054 = AXIS2_PLACEMENT_3D ( 'NONE', #4695, #4935, #17644 ) ;
#2055 = DIRECTION ( 'NONE',  ( -1.000000000000000000, 0.000000000000000000, 0.000000000000000000 ) ) ;
#2056 = CARTESIAN_POINT ( 'NONE',  ( 11.00000000000000000, 0.000000000000000000, 0.000000000000000000 ) ) ;
#2057 = CARTESIAN_POINT ( 'NONE',  ( 15.63975174930999934, -10.61757272617999881, 1.417689269007999853 ) ) ;
#2058 = CARTESIAN_POINT ( 'NONE',  ( -18.64256589945999920, -8.356153348075000764, -6.118136038720999537 ) ) ;
#2059 = CARTESIAN_POINT ( 'NONE',  ( 4.000000000000000000, 29.79977277844472994, 1.897803675662218970 ) ) ;
#2060 = CARTESIAN_POINT ( 'NONE',  ( -14.48091997122308783, 1.686280348617847258, 12.50000494027669262 ) ) ;
#2061 = ORIENTED_EDGE ( 'NONE', *, *, #22831, .F. ) ;
#2062 = CARTESIAN_POINT ( 'NONE',  ( -21.87664474417000093, 9.621532986476999838, 5.823833470188000128 ) ) ;
#2063 = CARTESIAN_POINT ( 'NONE',  ( 1.779182944342999839, 23.89536342497000021, 1.512334087421999929 ) ) ;
#2064 = CARTESIAN_POINT ( 'NONE',  ( 13.91722143161700487, -9.787662134382348000, 3.259115714080555559 ) ) ;
#2065 = LINE ( 'NONE', #14776, #23782 ) ;
#2066 = CARTESIAN_POINT ( 'NONE',  ( 24.56575753602000134, -0.1539563260370000186, 11.31598377959000068 ) ) ;
#2067 = EDGE_CURVE ( 'NONE', #22434, #744, #7596, .T. ) ;
#2068 = CARTESIAN_POINT ( 'NONE',  ( -1.911670502565000040, 29.90524234017999916, -1.384813786399999858 ) ) ;
#2069 = CARTESIAN_POINT ( 'NONE',  ( 13.80188479459891404, 9.025291018604240989, 0.006585034666644948471 ) ) ;
#2070 = CARTESIAN_POINT ( 'NONE',  ( 4.811303266717004590, 12.64225230711998549, 0.1541639457764001631 ) ) ;
#2071 = PRODUCT_DEFINITION_FORMATION_WITH_SPECIFIED_SOURCE ( 'ANY', '', #17128, .NOT_KNOWN. ) ;
#2072 = DIRECTION ( 'NONE',  ( 0.000000000000000000, 1.000000000000000000, 0.000000000000000000 ) ) ;
#2073 = CARTESIAN_POINT ( 'NONE',  ( 22.07140646839999931, 11.31094428649000072, 1.749821515072000011 ) ) ;
#2074 = ORIENTED_EDGE ( 'NONE', *, *, #499, .T. ) ;
#2075 = CARTESIAN_POINT ( 'NONE',  ( 0.6634078306992999829, 24.00000000000000000, -2.410371351092000403 ) ) ;
#2076 = VERTEX_POINT ( 'NONE', #2150 ) ;
#2077 = DIRECTION ( 'NONE',  ( 0.000000000000000000, 1.000000000000000000, 0.000000000000000000 ) ) ;
#2078 = AXIS2_PLACEMENT_3D ( 'NONE', #8810, #19713, #14251 ) ;
#2079 = DIRECTION ( 'NONE',  ( 0.000000000000000000, 0.000000000000000000, -1.000000000000000000 ) ) ;
#2080 = CARTESIAN_POINT ( 'NONE',  ( -2.000000000000000000, 28.00000000000000000, -3.464101615137999968 ) ) ;
#2081 = CARTESIAN_POINT ( 'NONE',  ( 18.05402034664000155, -0.4689034603063000350, -11.10308750183000015 ) ) ;
#2082 = DIRECTION ( 'NONE',  ( 0.000000000000000000, -1.000000000000000000, 0.000000000000000000 ) ) ;
#2083 = CARTESIAN_POINT ( 'NONE',  ( 2.628147087956000050, 27.85712896667000038, 0.4693273880717999669 ) ) ;
#2084 = ORIENTED_EDGE ( 'NONE', *, *, #954, .T. ) ;
#2085 = ORIENTED_EDGE ( 'NONE', *, *, #10886, .T. ) ;
#2086 = CARTESIAN_POINT ( 'NONE',  ( -12.53440221169000068, 2.913425087080000253, -14.82027568206000012 ) ) ;
#2087 = CARTESIAN_POINT ( 'NONE',  ( -2.100000000000000089, 18.89999999999999858, -1.955010042741999895E-10 ) ) ;
#2088 = AXIS2_PLACEMENT_3D ( 'NONE', #1850, #2082, #3907 ) ;
#2089 = CARTESIAN_POINT ( 'NONE',  ( 2.309807618587000011, 30.69019238141000017, -7.292675330123999428E-08 ) ) ;
#2090 = ORIENTED_EDGE ( 'NONE', *, *, #3850, .F. ) ;
#2091 = CARTESIAN_POINT ( 'NONE',  ( 1.699999999999999956, 9.063113307333603430, 0.9835126878571698317 ) ) ;
#2092 = CARTESIAN_POINT ( 'NONE',  ( 20.58645603379664379, -8.038508279625668607, -4.632961155938045472 ) ) ;
#2093 = DIRECTION ( 'NONE',  ( 0.000000000000000000, 0.000000000000000000, 1.000000000000000000 ) ) ;
#2094 = CARTESIAN_POINT ( 'NONE',  ( 15.93110892925370159, -9.670762698854872497, -3.710595638575625355 ) ) ;
#2095 = CARTESIAN_POINT ( 'NONE',  ( -18.05146424826999763, 4.664330861219999846, 10.07481800594999832 ) ) ;
#2096 = EDGE_CURVE ( 'NONE', #7720, #2709, #13864, .T. ) ;
#2097 = CARTESIAN_POINT ( 'NONE',  ( -1.709564223436000008, 30.70248379823999940, -1.373128400647000147 ) ) ;
#2098 = AXIS2_PLACEMENT_3D ( 'NONE', #6220, #15061, #20760 ) ;
#2099 = CARTESIAN_POINT ( 'NONE',  ( -14.57995894006000093, 5.497579849475999758, -8.642519878353001062 ) ) ;
#2100 = CARTESIAN_POINT ( 'NONE',  ( -0.1596195074772966960, 29.59450039907439844, 2.155456660100716793 ) ) ;
#2101 = ORIENTED_EDGE ( 'NONE', *, *, #16355, .F. ) ;
#2102 = CARTESIAN_POINT ( 'NONE',  ( 1.077617376005999938, 24.89850271714000129, 1.896742336415000008 ) ) ;
#2103 = CARTESIAN_POINT ( 'NONE',  ( 19.16431378521849993, -5.700780802628737653, 8.808059238752626641 ) ) ;
#2104 = CIRCLE ( 'NONE', #6368, 10.59999999999999964 ) ;
#2105 = CARTESIAN_POINT ( 'NONE',  ( -17.84889801066703541, -7.935400264423112304, 6.802475617916535988 ) ) ;
#2106 = ORIENTED_EDGE ( 'NONE', *, *, #14833, .F. ) ;
#2107 = CARTESIAN_POINT ( 'NONE',  ( 24.36414987671881605, -3.145589772712558574, 12.49999999999999822 ) ) ;
#2108 = CARTESIAN_POINT ( 'NONE',  ( 0.8814216895542995589, 30.38924864007917037, -2.379548453065109648 ) ) ;
#2109 = ADVANCED_FACE ( 'NONE', ( #9541 ), #4653, .F. ) ;
#2110 = CARTESIAN_POINT ( 'NONE',  ( 15.67012625730999886, 7.503068644359999873, -5.298384255253999697 ) ) ;
#2111 = ORIENTED_EDGE ( 'NONE', *, *, #19314, .T. ) ;
#2112 = CARTESIAN_POINT ( 'NONE',  ( -5.047512558650118386, 15.90113563435273392, 3.469625691324551120 ) ) ;
#2113 = ADVANCED_FACE ( 'NONE', ( #4452 ), #17013, .T. ) ;
#2114 = DIRECTION ( 'NONE',  ( 0.000000000000000000, 1.000000000000000000, 0.000000000000000000 ) ) ;
#2115 = VERTEX_POINT ( 'NONE', #8209 ) ;
#2116 = CARTESIAN_POINT ( 'NONE',  ( -22.97657263213626067, 8.792444840933823613, -3.354899762457558499 ) ) ;
#2117 = CARTESIAN_POINT ( 'NONE',  ( 0.7954828832003001393, 11.65690288844000122, 4.699030088164001917 ) ) ;
#2118 = AXIS2_PLACEMENT_3D ( 'NONE', #19864, #8964, #6539 ) ;
#2119 = B_SPLINE_CURVE_WITH_KNOTS ( 'NONE', 3,
 ( #12252, #19992, #19639, #8736, #19763, #16343, #21578, #10673, #14529, #6911 ),
 .UNSPECIFIED., .F., .F.,
 ( 4, 2, 2, 2, 4 ),
 ( 0.000000000000000000, 0.2500000000000000000, 0.5000000000000000000, 0.7500000000000000000, 1.000000000000000000 ),
 .UNSPECIFIED. ) ;
#2120 = CARTESIAN_POINT ( 'NONE',  ( 12.00000000000000000, -3.904004055809709328, -8.760530875779460658 ) ) ;
#2121 = EDGE_CURVE ( 'NONE', #1329, #12723, #11841, .T. ) ;
#2122 = CARTESIAN_POINT ( 'NONE',  ( -14.38789256606429312, 8.761241120844390551, -9.824672794992732605 ) ) ;
#2123 = DIRECTION ( 'NONE',  ( 0.000000000000000000, 1.000000000000000000, 0.000000000000000000 ) ) ;
#2124 = DIRECTION ( 'NONE',  ( 0.000000000000000000, 1.000000000000000000, 0.000000000000000000 ) ) ;
#2125 = CARTESIAN_POINT ( 'NONE',  ( 5.302306457911683424, 13.74700690846063722, -4.399542679587089111 ) ) ;
#2126 = FACE_BOUND ( 'NONE', #7482, .T. ) ;
#2127 = CARTESIAN_POINT ( 'NONE',  ( -0.7985131490157234557, 30.35564972260119632, 2.010576473712321288 ) ) ;
#2128 = ORIENTED_EDGE ( 'NONE', *, *, #12229, .T. ) ;
#2129 = CARTESIAN_POINT ( 'NONE',  ( -17.92162077250666030, -1.195142481609338336, -9.131185823717723693 ) ) ;
#2130 = CARTESIAN_POINT ( 'NONE',  ( 24.28529421024000001, -10.38286454550999949, -1.040937569600999923 ) ) ;
#2131 = CARTESIAN_POINT ( 'NONE',  ( 13.65567517025193922, 0.7181510411685014805, -9.045400155240761464 ) ) ;
#2132 = CARTESIAN_POINT ( 'NONE',  ( 2.500000000000001776, 27.81753006952333251, 0.3272492347489266429 ) ) ;
#2133 = CARTESIAN_POINT ( 'NONE',  ( -23.91099216809519490, 9.753959700133281174, -4.141585236787074464 ) ) ;
#2134 = CARTESIAN_POINT ( 'NONE',  ( 2.193490157264000207, 25.62614211381999851, -0.6650079486841000698 ) ) ;
#2135 = ADVANCED_FACE ( 'NONE', ( #8576 ), #23202, .T. ) ;
#2136 = CARTESIAN_POINT ( 'NONE',  ( -6.525832981339341643, 26.41017609473133732, 0.9999999999999872324 ) ) ;
#2137 = VERTEX_POINT ( 'NONE', #10030 ) ;
#2138 = CARTESIAN_POINT ( 'NONE',  ( -1.692126093021008471, 11.60421557973431383, -4.510750546857305920 ) ) ;
#2139 = CARTESIAN_POINT ( 'NONE',  ( -2.404489386789160132, 29.99040384242091406, 3.230569558791225315 ) ) ;
#2140 = CARTESIAN_POINT ( 'NONE',  ( 24.24531177150999994, 0.000000000000000000, 0.000000000000000000 ) ) ;
#2141 = EDGE_LOOP ( 'NONE', ( #9313, #22325, #20795, #1922, #9033, #14452, #2349 ) ) ;
#2142 = DIRECTION ( 'NONE',  ( -0.9989428060277519839, 0.000000000000000000, 0.04597031961386779941 ) ) ;
#2143 = CARTESIAN_POINT ( 'NONE',  ( 13.09050158531000108, 2.578416522421000057, 9.802228185182000786 ) ) ;
#2144 = EDGE_CURVE ( 'NONE', #551, #18791, #8909, .T. ) ;
#2145 = AXIS2_PLACEMENT_3D ( 'NONE', #20981, #620, #2700 ) ;
#2146 = CARTESIAN_POINT ( 'NONE',  ( -18.40696791751999584, 10.89439442848000006, 3.426539622133999874 ) ) ;
#2147 = FACE_OUTER_BOUND ( 'NONE', #21896, .T. ) ;
#2148 = EDGE_CURVE ( 'NONE', #5466, #3402, #11260, .T. ) ;
#2149 = CARTESIAN_POINT ( 'NONE',  ( 14.44733580085999947, 1.586710932958000031, -11.21110614856999987 ) ) ;
#2150 = CARTESIAN_POINT ( 'NONE',  ( 1.709999999999999964, 9.000000000000000000, 7.500000000000000000 ) ) ;
#2151 = CIRCLE ( 'NONE', #15677, 7.200000000000000178 ) ;
#2152 = FACE_BOUND ( 'NONE', #19736, .T. ) ;
#2153 = CARTESIAN_POINT ( 'NONE',  ( 23.32294689903000062, -6.854607272587000644, 7.667868601460999578 ) ) ;
#2154 = DIRECTION ( 'NONE',  ( -1.000000000000000000, 0.000000000000000000, 0.000000000000000000 ) ) ;
#2155 = VERTEX_POINT ( 'NONE', #19475 ) ;
#2156 = CARTESIAN_POINT ( 'NONE',  ( 0.000000000000000000, 18.27087121525220681, 0.000000000000000000 ) ) ;
#2157 = PLANE ( 'NONE',  #9897 ) ;
#2158 = CARTESIAN_POINT ( 'NONE',  ( -4.779708402705001191, 12.47950863541999311, -0.05972554645062000400 ) ) ;
#2159 = DIRECTION ( 'NONE',  ( -0.9996708941621511579, -0.02565352539213875543, 0.000000000000000000 ) ) ;
#2160 = CARTESIAN_POINT ( 'NONE',  ( -20.95361754275000266, -9.668541804323000477, -5.404777570993999802 ) ) ;
#2161 = ORIENTED_EDGE ( 'NONE', *, *, #5383, .T. ) ;
#2162 = ADVANCED_FACE ( 'NONE', ( #12208, #17533, #19597 ), #685, .T. ) ;
#2163 = EDGE_CURVE ( 'NONE', #19254, #13362, #7210, .T. ) ;
#2164 = ORIENTED_EDGE ( 'NONE', *, *, #16063, .T. ) ;
#2165 = CARTESIAN_POINT ( 'NONE',  ( 5.186887866327001717, 13.91948403396000344, 4.156460832888996926 ) ) ;
#2166 = CARTESIAN_POINT ( 'NONE',  ( 1.834054417453000019, 26.41049822781000245, 1.332518472557000067 ) ) ;
#2167 = DIRECTION ( 'NONE',  ( -1.000000000000000000, 0.000000000000000000, 0.000000000000000000 ) ) ;
#2168 = AXIS2_PLACEMENT_3D ( 'NONE', #21753, #12667, #21512 ) ;
#2169 = CARTESIAN_POINT ( 'NONE',  ( 24.00034722001000276, -13.93375672974000068, 0.2887811717300000081 ) ) ;
#2170 = CARTESIAN_POINT ( 'NONE',  ( -14.00000000000000000, 1.396097351027999937E-14, 0.000000000000000000 ) ) ;
#2171 =( NAMED_UNIT ( * ) PLANE_ANGLE_UNIT ( ) SI_UNIT ( $, .RADIAN. ) );
#2172 = CARTESIAN_POINT ( 'NONE',  ( -13.40193493347000064, -7.644751109369999575, -7.551345029496000727 ) ) ;
#2173 = CARTESIAN_POINT ( 'NONE',  ( 8.124934037954998800, 0.000000000000000000, 0.000000000000000000 ) ) ;
#2174 = CARTESIAN_POINT ( 'NONE',  ( -14.49454818139149559, 1.035381146816525266, 12.50000698751844297 ) ) ;
#2175 = ORIENTED_EDGE ( 'NONE', *, *, #6317, .F. ) ;
#2176 = CARTESIAN_POINT ( 'NONE',  ( 0.9165514763390999464, 25.32691554002000345, 2.353385513049000011 ) ) ;
#2177 = CARTESIAN_POINT ( 'NONE',  ( 13.95888961830255859, -10.15714629801752444, 1.812660213858063862 ) ) ;
#2178 = CARTESIAN_POINT ( 'NONE',  ( -17.80234587121333689, 8.890592914788218337, -2.389150121181911501 ) ) ;
#2179 = CARTESIAN_POINT ( 'NONE',  ( 23.68494808727000134, 6.489360873926000473, -9.241806053444001634 ) ) ;
#2180 = CARTESIAN_POINT ( 'NONE',  ( 1.582905715914000089, 28.79448331121999871, -2.003189615728000028 ) ) ;
#2181 = CARTESIAN_POINT ( 'NONE',  ( 14.53764925629900873, -7.579119239074397107, 5.000770392501714845 ) ) ;
#2182 = FACE_OUTER_BOUND ( 'NONE', #19800, .T. ) ;
#2183 = AXIS2_PLACEMENT_3D ( 'NONE', #972, #17326, #730 ) ;
#2184 = CARTESIAN_POINT ( 'NONE',  ( -6.809815940849730076, 15.32358591363257361, 1.841184338583090829 ) ) ;
#2185 = CARTESIAN_POINT ( 'NONE',  ( -0.6543697108982035049, 29.66753006952333038, -2.434931691670788823 ) ) ;
#2186 = ORIENTED_EDGE ( 'NONE', *, *, #15398, .F. ) ;
#2187 = CARTESIAN_POINT ( 'NONE',  ( -14.50561062189895267, 1.530330873916638801, -8.911763648040071928 ) ) ;
#2188 = CARTESIAN_POINT ( 'NONE',  ( 0.000000000000000000, 20.00000000000000000, 0.000000000000000000 ) ) ;
#2189 = ORIENTED_EDGE ( 'NONE', *, *, #3215, .T. ) ;
#2190 = CARTESIAN_POINT ( 'NONE',  ( 60.61494135913342518, 35.51856778792605240, 2.673746900119610359 ) ) ;
#2191 = DIRECTION ( 'NONE',  ( 1.000000000000000000, 0.000000000000000000, 0.000000000000000000 ) ) ;
#2192 = CARTESIAN_POINT ( 'NONE',  ( -4.000000000000000000, 28.30000000000000071, -2.309401076759000304 ) ) ;
#2193 = VECTOR ( 'NONE', #17019, 1000.000000000000000 ) ;
#2194 = ORIENTED_EDGE ( 'NONE', *, *, #2450, .T. ) ;
#2195 = CARTESIAN_POINT ( 'NONE',  ( 19.07657543443000137, -3.766769386410000031, 9.975653420128997695 ) ) ;
#2196 = DIRECTION ( 'NONE',  ( 0.000000000000000000, 0.000000000000000000, -1.000000000000000000 ) ) ;
#2197 = CIRCLE ( 'NONE', #23072, 4.750000000000000000 ) ;
#2198 = PRODUCT_DEFINITION ( 'UNKNOWN', '', #1306, #11213 ) ;
#2199 = CARTESIAN_POINT ( 'NONE',  ( 2.644546391786999795, 26.29712896667000166, -0.3657850755363000195 ) ) ;
#2200 = ORIENTED_EDGE ( 'NONE', *, *, #9489, .F. ) ;
#2201 = VERTEX_POINT ( 'NONE', #17784 ) ;
#2202 = CIRCLE ( 'NONE', #20008, 12.89775331292476857 ) ;
#2203 = CARTESIAN_POINT ( 'NONE',  ( -13.99999999999999467, 1.266994025276806379, -9.342908241774937395 ) ) ;
#2204 = CARTESIAN_POINT ( 'NONE',  ( -12.33813113877000056, 2.847851204958999460, -14.48670849514999937 ) ) ;
#2205 = DIRECTION ( 'NONE',  ( 0.000000000000000000, -1.000000000000000000, 0.000000000000000000 ) ) ;
#2206 = DIRECTION ( 'NONE',  ( -0.000000000000000000, 0.5000000000000169864, 0.8660254037844288266 ) ) ;
#2207 = ORIENTED_EDGE ( 'NONE', *, *, #196, .F. ) ;
#2208 = CARTESIAN_POINT ( 'NONE',  ( -14.49454820080683426, 11.34301321103429494, 5.353338751784230354 ) ) ;
#2209 = DIRECTION ( 'NONE',  ( 0.000000000000000000, 0.000000000000000000, 1.000000000000000000 ) ) ;
#2210 = CARTESIAN_POINT ( 'NONE',  ( 6.146042104385863070, 14.15896049273807300, 0.1829400497938399317 ) ) ;
#2211 = CARTESIAN_POINT ( 'NONE',  ( 15.47072016145524742, -3.491802273154016589, 9.789331991493677165 ) ) ;
#2212 = CARTESIAN_POINT ( 'NONE',  ( -13.74958640564999968, -10.81015631786999975, 1.945342028014000135 ) ) ;
#2213 = CARTESIAN_POINT ( 'NONE',  ( 2.066101926701000124, 28.83212126072000103, -0.7343076075657000157 ) ) ;
#2214 = VECTOR ( 'NONE', #16785, 1000.000000000000000 ) ;
#2215 = CARTESIAN_POINT ( 'NONE',  ( -18.11469101799999848, 6.086102628551000038, 9.654141096248000764 ) ) ;
#2216 = CARTESIAN_POINT ( 'NONE',  ( 0.9705800173758099003, 29.66328920622348164, 1.929470939684508446 ) ) ;
#2217 = EDGE_LOOP ( 'NONE', ( #14711, #832, #15805, #13513, #16578, #452, #4323, #22133, #17526, #4127 ) ) ;
#2218 = VECTOR ( 'NONE', #13396, 1000.000000000000000 ) ;
#2219 = CARTESIAN_POINT ( 'NONE',  ( -0.8426916045660000076, 24.46137432145000190, -2.178369093381999910 ) ) ;
#2220 = CARTESIAN_POINT ( 'NONE',  ( 19.27780731986851137, -8.649574563187062637, 5.948916446097893385 ) ) ;
#2221 = CARTESIAN_POINT ( 'NONE',  ( -1.500000000000000000, 8.900000000000000355, 0.000000000000000000 ) ) ;
#2222 = ORIENTED_EDGE ( 'NONE', *, *, #22126, .F. ) ;
#2223 = CARTESIAN_POINT ( 'NONE',  ( 6.642147790651000250, 13.49920969778000135, 0.06640950685239001283 ) ) ;
#2224 = CARTESIAN_POINT ( 'NONE',  ( -13.99999999999999645, -9.587150838885284188, 3.957974977218785551 ) ) ;
#2225 = EDGE_CURVE ( 'NONE', #19945, #23711, #22818, .T. ) ;
#2226 = CARTESIAN_POINT ( 'NONE',  ( 17.89031392131000331, 9.735558222862998434, -0.5785200253907000212 ) ) ;
#2227 = ORIENTED_EDGE ( 'NONE', *, *, #19457, .F. ) ;
#2228 = CIRCLE ( 'NONE', #13834, 4.000000000000000000 ) ;
#2229 = CARTESIAN_POINT ( 'NONE',  ( 0.000000000000000000, 24.50000000000000000, 4.618802153517000519 ) ) ;
#2230 = CARTESIAN_POINT ( 'NONE',  ( 24.36165043081783921, -12.41271798542465810, 3.500541789220333211 ) ) ;
#2231 = EDGE_LOOP ( 'NONE', ( #561, #23771, #16258, #1932 ) ) ;
#2232 = CARTESIAN_POINT ( 'NONE',  ( -16.78197087121331421, -9.101940161118450945, -1.191568128638077928 ) ) ;
#2233 = CARTESIAN_POINT ( 'NONE',  ( 21.70045833333333007, -5.671044614236272707, 7.379541929059594274 ) ) ;
#2234 = CARTESIAN_POINT ( 'NONE',  ( -1.890114362710001217, 11.79193194378000342, 4.373319237984003571 ) ) ;
#2235 = CARTESIAN_POINT ( 'NONE',  ( -23.10002682443999689, 8.026624707145000315, -5.342598563384999721 ) ) ;
#2236 = EDGE_CURVE ( 'NONE', #379, #2137, #16244, .T. ) ;
#2237 = LINE ( 'NONE', #22463, #21144 ) ;
#2238 = CARTESIAN_POINT ( 'NONE',  ( -4.544324455327999779, 13.49053734526000170, 5.132126114358000812 ) ) ;
#2239 = CARTESIAN_POINT ( 'NONE',  ( 2.171895212930905927, 26.39461574793667964, -0.7558918567651692344 ) ) ;
#2240 = CARTESIAN_POINT ( 'NONE',  ( 4.903707650242860261, 14.76847038361531794, 3.672007579896967577 ) ) ;
#2241 = DIRECTION ( 'NONE',  ( 1.000000000000000000, 0.000000000000000000, 0.000000000000000000 ) ) ;
#2242 = CARTESIAN_POINT ( 'NONE',  ( 2.161494655731827752, 30.60562575067124769, -0.02939362918790352705 ) ) ;
#2243 = ORIENTED_EDGE ( 'NONE', *, *, #13378, .T. ) ;
#2244 = CARTESIAN_POINT ( 'NONE',  ( -17.24137077250667005, 7.287857340677485141, 5.600902193946013519 ) ) ;
#2245 = CARTESIAN_POINT ( 'NONE',  ( 22.93253767531999898, 1.313452474455999885, -10.31494984694000117 ) ) ;
#2246 = CARTESIAN_POINT ( 'NONE',  ( 3.397923753680991421, 13.19211977465199581, -5.856784336400644442 ) ) ;
#2247 = LINE ( 'NONE', #19201, #23507 ) ;
#2248 = CIRCLE ( 'NONE', #18503, 10.59999999999999964 ) ;
#2249 = CARTESIAN_POINT ( 'NONE',  ( -21.55467116628538804, 1.019337657976560729, 10.62255827922021112 ) ) ;
#2250 = CARTESIAN_POINT ( 'NONE',  ( 2.249552142899000184, 25.59446440325999816, 0.5061648749511999945 ) ) ;
#2251 = LINE ( 'NONE', #16902, #21276 ) ;
#2252 = VERTEX_POINT ( 'NONE', #22223 ) ;
#2253 = AXIS2_PLACEMENT_3D ( 'NONE', #21946, #5588, #13090 ) ;
#2254 = EDGE_CURVE ( 'NONE', #12473, #8479, #9295, .T. ) ;
#2255 = DIRECTION ( 'NONE',  ( 0.000000000000000000, -1.000000000000000000, 0.000000000000000000 ) ) ;
#2256 = CARTESIAN_POINT ( 'NONE',  ( 24.39431354042982747, 9.829649394705615606, 2.587219325858395311E-05 ) ) ;
#2257 = CONICAL_SURFACE ( 'NONE', #7289, 4.309401076758999416, 1.119376321708719590 ) ;
#2258 = CONICAL_SURFACE ( 'NONE', #11158, 9.136555860486998526, 0.02565634000431304615 ) ;
#2259 = CARTESIAN_POINT ( 'NONE',  ( 1.120714571573853569, 28.16129399599262584, -1.892129278840122941 ) ) ;
#2260 = CARTESIAN_POINT ( 'NONE',  ( 6.243179582884000212, 13.63342035941999875, -1.952365010387999922 ) ) ;
#2261 = CARTESIAN_POINT ( 'NONE',  ( 0.000000000000000000, 20.10000000000000142, 0.000000000000000000 ) ) ;
#2262 = CIRCLE ( 'NONE', #11164, 1.500000000000001332 ) ;
#2263 = CARTESIAN_POINT ( 'NONE',  ( 17.28506424931000041, -8.106780832215999766, 7.067619055798999739 ) ) ;
#2264 = EDGE_CURVE ( 'NONE', #12880, #7614, #15467, .T. ) ;
#2265 = CARTESIAN_POINT ( 'NONE',  ( -15.76627339390999971, -11.34295740443999989, -0.3014791613419999794 ) ) ;
#2266 = CARTESIAN_POINT ( 'NONE',  ( -2.949999988794999695, 24.49999998879500041, -5.832343010994999544E-08 ) ) ;
#2267 = CARTESIAN_POINT ( 'NONE',  ( 13.02546080085999947, 11.25441903210000127, -0.8115343024272000383 ) ) ;
#2268 = DIRECTION ( 'NONE',  ( 0.000000000000000000, 1.000000000000000000, 0.000000000000000000 ) ) ;
#2269 = CARTESIAN_POINT ( 'NONE',  ( -6.042815635770000249, 16.39253429789999927, 0.9999999720525000191 ) ) ;
#2270 = CARTESIAN_POINT ( 'NONE',  ( 19.33361118158000025, -4.341085640097999132, 9.785006935544998896 ) ) ;
#2271 = AXIS2_PLACEMENT_3D ( 'NONE', #12296, #1151, #13730 ) ;
#2272 = CARTESIAN_POINT ( 'NONE',  ( 24.50000000000000711, -10.56912816078165562, 6.693733033818888956 ) ) ;
#2273 = VERTEX_POINT ( 'NONE', #5761 ) ;
#2274 = CARTESIAN_POINT ( 'NONE',  ( 12.12827354077999864, -2.665947717100999981, -8.940798416249000624 ) ) ;
#2275 = CARTESIAN_POINT ( 'NONE',  ( 0.4693273880718999980, 26.57706776951999927, 2.628147087956000050 ) ) ;
#2276 = VECTOR ( 'NONE', #589, 1000.000000000000114 ) ;
#2277 = CARTESIAN_POINT ( 'NONE',  ( 4.874073134685000142, 12.42371922698999853, 0.6764121694032001475 ) ) ;
#2278 = EDGE_CURVE ( 'NONE', #19420, #2511, #13558, .T. ) ;
#2279 = CARTESIAN_POINT ( 'NONE',  ( 1.892954172570674443, 28.93993560461466430, 1.040653877296049856 ) ) ;
#2280 = CARTESIAN_POINT ( 'NONE',  ( -20.76607004806999868, 1.065680277943000132, -11.02016022475999968 ) ) ;
#2281 = EDGE_LOOP ( 'NONE', ( #7740, #14456, #10120, #8642 ) ) ;
#2282 = CARTESIAN_POINT ( 'NONE',  ( 4.724999978625000097, 14.90000002138000035, 2.519183602109999904E-09 ) ) ;
#2283 = VECTOR ( 'NONE', #5334, 1000.000000000000114 ) ;
#2284 = ORIENTED_EDGE ( 'NONE', *, *, #20180, .T. ) ;
#2285 = ADVANCED_FACE ( 'NONE', ( #5636 ), #13021, .T. ) ;
#2286 = CARTESIAN_POINT ( 'NONE',  ( 4.622963014007718918, 12.49839699622550349, 1.256155413754589167 ) ) ;
#2287 = CARTESIAN_POINT ( 'NONE',  ( 2.070238309910999774, 25.66299822781000017, 0.4658180156273000194 ) ) ;
#2288 = CARTESIAN_POINT ( 'NONE',  ( 24.50000000000000000, 0.000000000000000000, 0.000000000000000000 ) ) ;
#2289 = EDGE_CURVE ( 'NONE', #20328, #13328, #20422, .T. ) ;
#2290 = DIRECTION ( 'NONE',  ( 1.000000000000000000, 0.000000000000000000, 0.000000000000000000 ) ) ;
#2291 = CARTESIAN_POINT ( 'NONE',  ( 13.22662674931000204, 6.334720884006999952, 8.559150566242998082 ) ) ;
#2292 = CIRCLE ( 'NONE', #1916, 0.9999989211906009645 ) ;
#2293 = CARTESIAN_POINT ( 'NONE',  ( -12.79254388956000099, 9.568035197138000214, -2.460455418527999871 ) ) ;
#2294 = AXIS2_PLACEMENT_3D ( 'NONE', #15694, #23084, #6509 ) ;
#2295 = FACE_OUTER_BOUND ( 'NONE', #18594, .T. ) ;
#2296 = AXIS2_PLACEMENT_3D ( 'NONE', #19510, #17569, #10301 ) ;
#2297 = CARTESIAN_POINT ( 'NONE',  ( -14.33281117769207569, -5.151946275727822488, 12.49999999999962697 ) ) ;
#2298 = ORIENTED_EDGE ( 'NONE', *, *, #3038, .T. ) ;
#2299 = EDGE_CURVE ( 'NONE', #6464, #386, #4181, .T. ) ;
#2300 = SURFACE_STYLE_FILL_AREA ( #2533 ) ;
#2301 = EDGE_CURVE ( 'NONE', #19402, #8374, #11997, .T. ) ;
#2302 = CARTESIAN_POINT ( 'NONE',  ( -0.3250653824660000302, 23.76728119616999635, 2.312349103826000007 ) ) ;
#2303 = CARTESIAN_POINT ( 'NONE',  ( 13.84539632146338128, -8.680774802907970766, 5.550785524995694331 ) ) ;
#2304 = EDGE_LOOP ( 'NONE', ( #3750, #2061, #10700, #16455 ) ) ;
#2305 = CARTESIAN_POINT ( 'NONE',  ( -2.461267912185001183, 12.87788887804001803, -6.662423917068999835 ) ) ;
#2306 = CARTESIAN_POINT ( 'NONE',  ( -2.067612397392999846, 29.79980770961000047, -1.497778068447999766 ) ) ;
#2307 = CARTESIAN_POINT ( 'NONE',  ( 12.28779254564781986, -5.665119685639886882, 12.50001287414623619 ) ) ;
#2308 = CARTESIAN_POINT ( 'NONE',  ( 18.71311277160243947, 3.105602819214801080, 10.00188426715560297 ) ) ;
#2309 = CARTESIAN_POINT ( 'NONE',  ( -12.25000000000000000, 1.374666032043000015E-14, 0.000000000000000000 ) ) ;
#2310 = CARTESIAN_POINT ( 'NONE',  ( 11.85409292833900707, 8.571431512452234003, -10.15389364929188609 ) ) ;
#2311 = ORIENTED_EDGE ( 'NONE', *, *, #8685, .F. ) ;
#2312 = CARTESIAN_POINT ( 'NONE',  ( -1.835060406388425269, 24.49999999999985079, -3.559329533909751486 ) ) ;
#2313 = DIRECTION ( 'NONE',  ( 1.160410698086937980E-09, 2.689654613662110334E-16, 1.000000000000000000 ) ) ;
#2314 = ORIENTED_EDGE ( 'NONE', *, *, #6712, .T. ) ;
#2315 = CARTESIAN_POINT ( 'NONE',  ( 1.383873339091999943, 25.12749250491000197, 2.361535497914000192 ) ) ;
#2316 = CARTESIAN_POINT ( 'NONE',  ( -9.042815982636001948, 20.50000000000000000, -1.000000000000000000 ) ) ;
#2317 = CARTESIAN_POINT ( 'NONE',  ( 23.01485185659291233, 37.01856778792605240, -6.000000000000000000 ) ) ;
#2318 = ORIENTED_EDGE ( 'NONE', *, *, #537, .T. ) ;
#2319 = AXIS2_PLACEMENT_3D ( 'NONE', #1577, #3400, #11124 ) ;
#2320 = CARTESIAN_POINT ( 'NONE',  ( 15.88860957249000094, -10.52205501482999850, -3.386765196271000367 ) ) ;
#2321 = DIRECTION ( 'NONE',  ( 0.000000000000000000, 0.8660254037844288266, -0.5000000000000169864 ) ) ;
#2322 = CARTESIAN_POINT ( 'NONE',  ( 24.40278699097224901, -2.659935282767429854, -12.50000000000000178 ) ) ;
#2323 = VERTEX_POINT ( 'NONE', #2011 ) ;
#2324 = VERTEX_POINT ( 'NONE', #18713 ) ;
#2325 = CARTESIAN_POINT ( 'NONE',  ( -14.00000000000000178, -1.971496140865625302, -9.404298541413128376 ) ) ;
#2326 = CARTESIAN_POINT ( 'NONE',  ( -10.39612971169000133, 4.211105248640000021, 14.98851321108000079 ) ) ;
#2327 = CARTESIAN_POINT ( 'NONE',  ( 0.7010477225544974322, 6.813607535519789593, -1.604763118501952412 ) ) ;
#2328 = B_SPLINE_CURVE_WITH_KNOTS ( 'NONE', 3,
 ( #7721, #18622, #13278, #14853 ),
 .UNSPECIFIED., .F., .F.,
 ( 4, 4 ),
 ( 0.2478303497282951795, 0.2499810176238006776 ),
 .UNSPECIFIED. ) ;
#2329 = DIRECTION ( 'NONE',  ( 6.613961328593999866E-09, -8.164805666996911273E-09, 1.000000000000000000 ) ) ;
#2330 = ORIENTED_EDGE ( 'NONE', *, *, #16321, .T. ) ;
#2331 = ADVANCED_FACE ( 'NONE', ( #11578, #9396 ), #20540, .T. ) ;
#2332 = CARTESIAN_POINT ( 'NONE',  ( -23.10253524184999918, 6.427000661414000504, 7.964584163192999000 ) ) ;
#2333 = CARTESIAN_POINT ( 'NONE',  ( -14.39391696178813262, 8.762017990479289864, 9.823718642491295228 ) ) ;
#2334 = CARTESIAN_POINT ( 'NONE',  ( 0.000000000000000000, 21.89999999999999858, 0.000000000000000000 ) ) ;
#2335 = CARTESIAN_POINT ( 'NONE',  ( 15.31019486909626082, 2.146509511632994638, 10.14207265829758597 ) ) ;
#2336 = B_SPLINE_CURVE_WITH_KNOTS ( 'NONE', 3,
 ( #16007, #9005, #1254, #5140, #21954, #17974, #3443, #6946, #16375, #2956, #6695, #16130 ),
 .UNSPECIFIED., .F., .F.,
 ( 4, 1, 1, 1, 1, 1, 1, 1, 1, 4 ),
 ( 0.000000000000000000, 0.03719136591632924566, 0.1695487139369214469, 0.3019060619569148285, 0.4342634099775076750, 0.5666207579975004460, 0.6989781060180932926, 0.8313354540380859525, 0.9636928020586794652, 1.000000000000000000 ),
 .UNSPECIFIED. ) ;
#2337 = CARTESIAN_POINT ( 'NONE',  ( -14.00878788127999997, -9.282977100841998563, -4.456265381222999977 ) ) ;
#2338 = CARTESIAN_POINT ( 'NONE',  ( 2.306909816657999990, 30.44805800497999826, -0.4795071306118000032 ) ) ;
#2339 = CARTESIAN_POINT ( 'NONE',  ( -14.82384736926000102, 5.788590216149999357, -9.100136119003000346 ) ) ;
#2340 = CARTESIAN_POINT ( 'NONE',  ( 0.2739778719191235945, 29.61987499151109304, 2.142736234137259999 ) ) ;
#2341 = ORIENTED_EDGE ( 'NONE', *, *, #9075, .T. ) ;
#2342 = CARTESIAN_POINT ( 'NONE',  ( -2.162054140341999720, 23.60745938542000388, 0.3218784743804999904 ) ) ;
#2343 = CARTESIAN_POINT ( 'NONE',  ( -19.52737009387375267, -10.18506149564973207, 2.517846037059293440 ) ) ;
#2344 = ORIENTED_EDGE ( 'NONE', *, *, #3639, .F. ) ;
#2345 = CARTESIAN_POINT ( 'NONE',  ( -1.395367521490594731, 24.57895749046196343, -1.860951888388887143 ) ) ;
#2346 = CARTESIAN_POINT ( 'NONE',  ( -4.108124441661001214, 14.09331144393998692, 4.413805377952999542 ) ) ;
#2347 = CARTESIAN_POINT ( 'NONE',  ( 18.33699999999999974, -9.141845273363999880, 1.095420050962999850E-14 ) ) ;
#2348 = CARTESIAN_POINT ( 'NONE',  ( 14.59968892130999940, 4.304969983318999383, 8.654667617400001234 ) ) ;
#2349 = ORIENTED_EDGE ( 'NONE', *, *, #11203, .T. ) ;
#2350 = DIRECTION ( 'NONE',  ( 0.000000000000000000, -1.000000000000000000, 0.000000000000000000 ) ) ;
#2351 = CARTESIAN_POINT ( 'NONE',  ( 1.709999999999999964, 9.000000000000000000, -7.500000000000000000 ) ) ;
#2352 = ORIENTED_EDGE ( 'NONE', *, *, #23275, .T. ) ;
#2353 = CARTESIAN_POINT ( 'NONE',  ( 3.000000000000000000, 15.09999999999999964, 0.000000000000000000 ) ) ;
#2354 = DIRECTION ( 'NONE',  ( 0.000000000000000000, -1.000000000000000000, 0.000000000000000000 ) ) ;
#2355 = CARTESIAN_POINT ( 'NONE',  ( -4.724251990381001853, 12.60843673673999810, 0.4143338360902000250 ) ) ;
#2356 = DIRECTION ( 'NONE',  ( -1.387778780781444413E-14, 1.000000000000000000, 0.000000000000000000 ) ) ;
#2357 = CARTESIAN_POINT ( 'NONE',  ( -21.17298660481999661, 9.406917137533000073, -1.865098543902999895 ) ) ;
#2358 = DIRECTION ( 'NONE',  ( 0.000000000000000000, -1.000000000000000000, 0.000000000000000000 ) ) ;
#2359 = CARTESIAN_POINT ( 'NONE',  ( -3.317489423066998455, 13.45101538807001873, -5.148797630174996698 ) ) ;
#2360 = CARTESIAN_POINT ( 'NONE',  ( 5.972539995960000070, 13.70650976685000089, 2.690923256664000007 ) ) ;
#2361 = CARTESIAN_POINT ( 'NONE',  ( 5.302309017544000191, 13.73032573480000096, -4.450985556070999216 ) ) ;
#2362 = DIRECTION ( 'NONE',  ( 1.000000000000000000, 0.000000000000000000, 0.000000000000000000 ) ) ;
#2363 = EDGE_CURVE ( 'NONE', #3402, #12394, #8689, .T. ) ;
#2364 = CARTESIAN_POINT ( 'NONE',  ( 0.5181440266930791294, 30.43466978169055182, 2.096986438083043858 ) ) ;
#2365 = ORIENTED_EDGE ( 'NONE', *, *, #15909, .T. ) ;
#2366 = CARTESIAN_POINT ( 'NONE',  ( -16.90124577250666604, -2.383332030605061380, 8.867973604693034417 ) ) ;
#2367 = CARTESIAN_POINT ( 'NONE',  ( 18.82170634012999955, -6.238070653312000502, -7.492020000904000554 ) ) ;
#2368 = CARTESIAN_POINT ( 'NONE',  ( 3.914845617362098018, 13.31586473120900393, -5.570899607885616334 ) ) ;
#2369 = CARTESIAN_POINT ( 'NONE',  ( 2.000000000000000000, 30.00000000000000000, 3.464101615137999968 ) ) ;
#2370 = CARTESIAN_POINT ( 'NONE',  ( -22.86671354229583031, -10.53743997464867732, -0.7811924423727086841 ) ) ;
#2371 = CARTESIAN_POINT ( 'NONE',  ( -1.743177805438000050, 26.69864211382000008, -1.488814495283000028 ) ) ;
#2372 = B_SPLINE_CURVE_WITH_KNOTS ( 'NONE', 3,
 ( #6836, #20044, #21624, #17874, #23298, #18228, #4911, #10952, #14351, #10488 ),
 .UNSPECIFIED., .F., .F.,
 ( 4, 2, 2, 2, 4 ),
 ( 0.000000000000000000, 0.2500000000000000000, 0.5000000000000000000, 0.7500000000000000000, 1.000000000000000000 ),
 .UNSPECIFIED. ) ;
#2373 = DIRECTION ( 'NONE',  ( 0.000000000000000000, 0.000000000000000000, -1.000000000000000000 ) ) ;
#2374 = VERTEX_POINT ( 'NONE', #18954 ) ;
#2375 = CARTESIAN_POINT ( 'NONE',  ( -17.90765081723635177, 0.2656351261378813722, 10.58437225064310816 ) ) ;
#2376 = EDGE_CURVE ( 'NONE', #7890, #4095, #20895, .T. ) ;
#2377 = DIRECTION ( 'NONE',  ( -1.000000000000000000, 0.000000000000000000, 0.000000000000000000 ) ) ;
#2378 = LINE ( 'NONE', #23070, #4525 ) ;
#2379 = CARTESIAN_POINT ( 'NONE',  ( -14.03310205518379128, 8.843032913246654303, 2.087261342718107482 ) ) ;
#2380 = VERTEX_POINT ( 'NONE', #5875 ) ;
#2381 = CARTESIAN_POINT ( 'NONE',  ( 17.44974770046333390, 5.604008867033932972, -7.292312980387861465 ) ) ;
#2382 = CARTESIAN_POINT ( 'NONE',  ( 16.40756424930999913, 8.766565845128001300, -6.190543086277999763 ) ) ;
#2383 = CARTESIAN_POINT ( 'NONE',  ( -16.17253408984999652, -2.147297115180999860, 11.15346350841000067 ) ) ;
#2384 = CARTESIAN_POINT ( 'NONE',  ( 0.000000000000000000, 17.00000000000000000, 0.000000000000000000 ) ) ;
#2385 = CARTESIAN_POINT ( 'NONE',  ( 12.89051537305999950, 0.9064800472110999818, -9.847992809938999059 ) ) ;
#2386 = FACE_OUTER_BOUND ( 'NONE', #10840, .T. ) ;
#2387 = CARTESIAN_POINT ( 'NONE',  ( 2.434931691670791487, 27.00086340285667319, 0.6543697108981911814 ) ) ;
#2388 = CARTESIAN_POINT ( 'NONE',  ( 22.26065228610000091, 1.952640354001999867, -10.06840971000000096 ) ) ;
#2389 = EDGE_CURVE ( 'NONE', #16978, #15685, #5755, .T. ) ;
#2390 = AXIS2_PLACEMENT_3D ( 'NONE', #12324, #19715, #23689 ) ;
#2391 = DIRECTION ( 'NONE',  ( 0.000000000000000000, 0.000000000000000000, -1.000000000000000000 ) ) ;
#2392 = VERTEX_POINT ( 'NONE', #21012 ) ;
#2393 = FACE_OUTER_BOUND ( 'NONE', #1763, .T. ) ;
#2394 = CARTESIAN_POINT ( 'NONE',  ( 0.5485649090616000478, 28.98206776952000041, 2.437990915149000237 ) ) ;
#2395 = CARTESIAN_POINT ( 'NONE',  ( 2.814154119931001841, 11.91260811072999104, 3.809416604937000184 ) ) ;
#2396 = CARTESIAN_POINT ( 'NONE',  ( 2.066277796575604953, 28.96607617505452836, 0.6292312681296344801 ) ) ;
#2397 = CARTESIAN_POINT ( 'NONE',  ( -22.43691550588000183, 6.205779378985000427, -9.223551109405999426 ) ) ;
#2398 = EDGE_LOOP ( 'NONE', ( #12358, #4368, #19153, #3844 ) ) ;
#2399 = CARTESIAN_POINT ( 'NONE',  ( -6.637070260807000466, 26.35799170939839797, 1.000000000000000000 ) ) ;
#2400 = EDGE_LOOP ( 'NONE', ( #6111, #10554, #8252, #16567, #10570 ) ) ;
#2401 = FACE_OUTER_BOUND ( 'NONE', #16062, .T. ) ;
#2403 = EDGE_CURVE ( 'NONE', #4084, #18848, #2605, .T. ) ;
#2402 = CARTESIAN_POINT ( 'NONE',  ( -1.289728978252000058, 28.25506359723999950, -2.104626470933999904 ) ) ;
#2404 = CARTESIAN_POINT ( 'NONE',  ( 2.428345707995998470, 12.87484077716998598, 6.668354174382002064 ) ) ;
#2405 = DIRECTION ( 'NONE',  ( 0.000000000000000000, 0.7071067811866525998, -0.7071067811864425456 ) ) ;
#2406 = CARTESIAN_POINT ( 'NONE',  ( 12.34912674931000076, -5.416870430593999863, -9.140812312194999123 ) ) ;
#2407 = CARTESIAN_POINT ( 'NONE',  ( -16.81439276773000202, -8.006006257143999605, -6.488443847660000152 ) ) ;
#2408 = CIRCLE ( 'NONE', #15543, 4.000000000000000000 ) ;
#2409 = CARTESIAN_POINT ( 'NONE',  ( 14.46356375731000021, 0.7465905146449000052, 9.123040730097999429 ) ) ;
#2410 = EDGE_CURVE ( 'NONE', #16380, #6198, #13737, .T. ) ;
#2411 = CARTESIAN_POINT ( 'NONE',  ( -14.49284521823309824, -1.036537809018404310, 12.49997544921124337 ) ) ;
#2412 = ORIENTED_EDGE ( 'NONE', *, *, #20628, .F. ) ;
#2413 = CARTESIAN_POINT ( 'NONE',  ( 1.032299669828999900, 30.21051138681000126, -2.520645439494999973 ) ) ;
#2414 = CARTESIAN_POINT ( 'NONE',  ( 0.8975247896630000888, 23.72588767999999959, 2.360713936347000441 ) ) ;
#2415 = CARTESIAN_POINT ( 'NONE',  ( 13.83037995398642295, -8.404022434966693211, 5.981951882901380024 ) ) ;
#2416 = EDGE_LOOP ( 'NONE', ( #22277, #16261, #11059 ) ) ;
#2417 = CARTESIAN_POINT ( 'NONE',  ( -3.448929114309002397, 13.22474374734999003, -5.490345264048999141 ) ) ;
#2418 = CARTESIAN_POINT ( 'NONE',  ( 2.399999988616999591, 28.00000001138332806, 6.337991288364001799E-08 ) ) ;
#2419 = EDGE_CURVE ( 'NONE', #6719, #259, #2482, .T. ) ;
#2420 = CARTESIAN_POINT ( 'NONE',  ( -19.10482910584000038, 1.458613477275000161E-14, 0.000000000000000000 ) ) ;
#2421 = CARTESIAN_POINT ( 'NONE',  ( 11.90008533512006572, -4.641570061506480549, 12.50003962888516895 ) ) ;
#2422 = EDGE_CURVE ( 'NONE', #14961, #12189, #10707, .T. ) ;
#2423 = CARTESIAN_POINT ( 'NONE',  ( 18.04406002188076741, 5.225631352894819059, -9.061601784925585434 ) ) ;
#2424 = DIRECTION ( 'NONE',  ( 0.000000000000000000, -1.000000000000000000, 0.000000000000000000 ) ) ;
#2425 = DIRECTION ( 'NONE',  ( 0.9063077870366409439, 0.000000000000000000, -0.4226182617407189257 ) ) ;
#2426 = CARTESIAN_POINT ( 'NONE',  ( 11.72559253309100313, 8.766982473631962591, -9.815058144992619305 ) ) ;
#2427 = ORIENTED_EDGE ( 'NONE', *, *, #22115, .T. ) ;
#2428 = VECTOR ( 'NONE', #22513, 1000.000000000000000 ) ;
#2429 = CARTESIAN_POINT ( 'NONE',  ( -3.649794085728321758, 28.20197603011191134, 2.511592555635382418 ) ) ;
#2430 = VERTEX_POINT ( 'NONE', #12061 ) ;
#2431 = FACE_OUTER_BOUND ( 'NONE', #1149, .T. ) ;
#2433 = CARTESIAN_POINT ( 'NONE',  ( -1.269269236459868555, 23.68265782431019773, -1.789285403925672036 ) ) ;
#2432 = CARTESIAN_POINT ( 'NONE',  ( -3.066980279242876861, 11.87898535859614135, 3.727226793947211014 ) ) ;
#2434 = ADVANCED_FACE ( 'NONE', ( #19325 ), #5951, .T. ) ;
#2435 = FACE_OUTER_BOUND ( 'NONE', #12405, .T. ) ;
#2436 = DIRECTION ( 'NONE',  ( -1.000000000000000000, 0.000000000000000000, 0.000000000000000000 ) ) ;
#2437 = CARTESIAN_POINT ( 'NONE',  ( -7.135193656722003119, 15.40309895115001737, -1.043051061229000265 ) ) ;
#2438 = CARTESIAN_POINT ( 'NONE',  ( -1.150230160948066294, 26.50000000000000711, 2.153661957585351505 ) ) ;
#2439 = ORIENTED_EDGE ( 'NONE', *, *, #21974, .F. ) ;
#2440 = ORIENTED_EDGE ( 'NONE', *, *, #9146, .T. ) ;
#2441 = CARTESIAN_POINT ( 'NONE',  ( -13.99999999999999645, 1.449170934955976486, -9.306736692574475001 ) ) ;
#2442 = CARTESIAN_POINT ( 'NONE',  ( 2.404489386789160132, 29.99040384242091406, -3.230569558791225315 ) ) ;
#2443 = CARTESIAN_POINT ( 'NONE',  ( -14.48633706258206288, -10.11155074088070371, -7.486293916572105189 ) ) ;
#2444 = ORIENTED_EDGE ( 'NONE', *, *, #3636, .F. ) ;
#2445 = CARTESIAN_POINT ( 'NONE',  ( -22.24570156380999819, -7.689645674130000330, -6.718150816083000798 ) ) ;
#2446 = CARTESIAN_POINT ( 'NONE',  ( -24.16119556689726977, 8.771053125571407705, 9.807567373710691427 ) ) ;
#2447 = CARTESIAN_POINT ( 'NONE',  ( 6.230117939712608965, 13.73923584163333800, 1.395535972837913308 ) ) ;
#2448 = CARTESIAN_POINT ( 'NONE',  ( 15.79764610807505143, -10.31663114728906905, 0.9025345700017101125 ) ) ;
#2449 = CARTESIAN_POINT ( 'NONE',  ( -18.34470744204000070, 4.667706239444999738, 10.08210694793999984 ) ) ;
#2450 = EDGE_CURVE ( 'NONE', #4848, #9355, #11382, .T. ) ;
#2451 = CARTESIAN_POINT ( 'NONE',  ( 0.1768883900467000114, 30.19892465351999888, 2.185563631071000046 ) ) ;
#2452 = CARTESIAN_POINT ( 'NONE',  ( -18.66670768690667614, -9.150306222430156566, 1.044069867951560981 ) ) ;
#2453 = EDGE_CURVE ( 'NONE', #14911, #6411, #12164, .T. ) ;
#2454 = CARTESIAN_POINT ( 'NONE',  ( -13.15804650426999878, -7.258886979407000339, -7.170289537978000283 ) ) ;
#2455 = CARTESIAN_POINT ( 'NONE',  ( 1.625795934526099940, 29.71217265414515651, 1.423553400153898085 ) ) ;
#2456 = ORIENTED_EDGE ( 'NONE', *, *, #21732, .T. ) ;
#2457 = CARTESIAN_POINT ( 'NONE',  ( -0.06890087385339001280, 24.58462810240999730, 2.184803246612999850 ) ) ;
#2458 = CARTESIAN_POINT ( 'NONE',  ( -19.18010000769303502, -6.003056531568853771, -8.588473314997994379 ) ) ;
#2459 = VERTEX_POINT ( 'NONE', #15794 ) ;
#2460 = CARTESIAN_POINT ( 'NONE',  ( 1.709999999999999964, 9.852710287022999225, -7.500000000000000000 ) ) ;
#2461 = CARTESIAN_POINT ( 'NONE',  ( -2.100000000000000089, 19.00000000000000000, 0.000000000000000000 ) ) ;
#2462 = EDGE_CURVE ( 'NONE', #2559, #19778, #13680, .T. ) ;
#2463 = CARTESIAN_POINT ( 'NONE',  ( -2.153985071724999756, 30.83999999999999986, 0.1610847937796999751 ) ) ;
#2464 = EDGE_CURVE ( 'NONE', #9388, #17324, #13862, .T. ) ;
#2465 = CARTESIAN_POINT ( 'NONE',  ( 8.196152422706999729, 26.90192378864669820, -6.000000000000000000 ) ) ;
#2466 = VECTOR ( 'NONE', #17383, 1000.000000000000000 ) ;
#2467 = CARTESIAN_POINT ( 'NONE',  ( 11.74781392131000146, -7.601052271439000307, -5.849495945765999849 ) ) ;
#2468 = VERTEX_POINT ( 'NONE', #8301 ) ;
#2469 = CARTESIAN_POINT ( 'NONE',  ( -6.230543946801002875, 16.13931437111000733, -0.9718497405647000820 ) ) ;
#2470 = DIRECTION ( 'NONE',  ( -1.280113743563924749E-07, -4.045642977578689132E-08, -0.9999999999999911182 ) ) ;
#2471 = DIRECTION ( 'NONE',  ( -1.000000000000000000, 0.000000000000000000, 0.000000000000000000 ) ) ;
#2472 = ORIENTED_EDGE ( 'NONE', *, *, #2718, .T. ) ;
#2473 = AXIS2_PLACEMENT_3D ( 'NONE', #2819, #1359, #21464 ) ;
#2474 = CARTESIAN_POINT ( 'NONE',  ( 0.000000000000000000, 30.84509624898000268, 0.000000000000000000 ) ) ;
#2475 = CARTESIAN_POINT ( 'NONE',  ( 3.000000000000000000, 17.89999999999999858, 0.000000000000000000 ) ) ;
#2476 = CARTESIAN_POINT ( 'NONE',  ( -1.058805613176999616, 11.70499902296001160, 4.728261420812001958 ) ) ;
#2477 = CARTESIAN_POINT ( 'NONE',  ( -12.50000000000000000, 6.992973968623999781, -5.709239639804999378 ) ) ;
#2478 = CARTESIAN_POINT ( 'NONE',  ( 17.68641176306230989, -10.25162057640060631, -1.802399854559492587 ) ) ;
#2479 = FACE_OUTER_BOUND ( 'NONE', #15038, .T. ) ;
#2480 = CARTESIAN_POINT ( 'NONE',  ( -14.25243324638999809, 7.716878364870000340, -11.63397459621999985 ) ) ;
#2481 = CARTESIAN_POINT ( 'NONE',  ( -4.724624249661752984, 13.39762491672413525, 5.370412594684863095 ) ) ;
#2482 = LINE ( 'NONE', #13614, #6338 ) ;
#2483 = CARTESIAN_POINT ( 'NONE',  ( 5.896080086043998136, 14.43358657436269432, 1.669016364038776956 ) ) ;
#2484 = CARTESIAN_POINT ( 'NONE',  ( 0.6543697108981985089, 28.00086340285666964, -2.434931691670790599 ) ) ;
#2485 = CARTESIAN_POINT ( 'NONE',  ( 1.613055828956475368, 30.51051290257240822, 1.451212359496641291 ) ) ;
#2486 = ORIENTED_EDGE ( 'NONE', *, *, #17155, .F. ) ;
#2487 = CARTESIAN_POINT ( 'NONE',  ( -17.05241243917333804, 2.384112843373643820, 8.871849034729358152 ) ) ;
#2488 = CARTESIAN_POINT ( 'NONE',  ( 20.56096474217000036, -7.987351613630001346, -5.673264839440999907 ) ) ;
#2489 = CARTESIAN_POINT ( 'NONE',  ( 2.198509335874302195, 12.96754872753050769, -6.338474540310088834 ) ) ;
#2490 = FACE_OUTER_BOUND ( 'NONE', #18572, .T. ) ;
#2491 = CARTESIAN_POINT ( 'NONE',  ( 1.990650851275000299, 25.56196440326000285, 1.014287269782000012 ) ) ;
#2492 = LINE ( 'NONE', #11707, #1148 ) ;
#2493 = ORIENTED_EDGE ( 'NONE', *, *, #14178, .T. ) ;
#2494 = CARTESIAN_POINT ( 'NONE',  ( 0.000000000000000000, 26.35000000000000142, 0.000000000000000000 ) ) ;
#2495 = FACE_OUTER_BOUND ( 'NONE', #23239, .T. ) ;
#2496 = CARTESIAN_POINT ( 'NONE',  ( -2.999999956181000016, 17.90000004382000043, 2.609181505839000138E-08 ) ) ;
#2497 = DIRECTION ( 'NONE',  ( 0.000000000000000000, 1.000000000000000000, 0.000000000000000000 ) ) ;
#2498 = ADVANCED_FACE ( 'NONE', ( #781 ), #8670, .T. ) ;
#2499 = ORIENTED_EDGE ( 'NONE', *, *, #4500, .T. ) ;
#2500 = CARTESIAN_POINT ( 'NONE',  ( 17.07183103379666633, -5.598228470880529883, -7.284378211082013443 ) ) ;
#2501 = AXIS2_PLACEMENT_3D ( 'NONE', #7515, #2425, #9577 ) ;
#2502 = CARTESIAN_POINT ( 'NONE',  ( 17.83350174931000254, -4.076359992019000344, -9.968186170592000295 ) ) ;
#2503 = CARTESIAN_POINT ( 'NONE',  ( -23.84635873346000068, 3.413845864946000397, 10.14151937845999996 ) ) ;
#2504 = CARTESIAN_POINT ( 'NONE',  ( 2.000000000000198508, 24.49999999999999645, -3.464101615138341028 ) ) ;
#2505 = CARTESIAN_POINT ( 'NONE',  ( 24.00016455292000117, -6.692834685703999753, -6.438753808737999407 ) ) ;
#2506 = CARTESIAN_POINT ( 'NONE',  ( 19.32280703972000069, -3.872993065167000371, 9.573872678542000969 ) ) ;
#2507 = CARTESIAN_POINT ( 'NONE',  ( -2.015949060104638590, 30.88564367501877683, -0.6669719759398144987 ) ) ;
#2508 = FACE_OUTER_BOUND ( 'NONE', #19005, .T. ) ;
#2509 = CARTESIAN_POINT ( 'NONE',  ( 19.48688301901000131, -0.05922813441184000827, 9.759376508132000083 ) ) ;
#2510 = CARTESIAN_POINT ( 'NONE',  ( 0.000000000000000000, -1.550000000000000044, 0.000000000000000000 ) ) ;
#2511 = VERTEX_POINT ( 'NONE', #6603 ) ;
#2512 = DIRECTION ( 'NONE',  ( 0.000000000000000000, 1.000000000000000000, 0.000000000000000000 ) ) ;
#2513 = CARTESIAN_POINT ( 'NONE',  ( 0.5721489135196999865, 28.52706776951999856, -2.607696352436000176 ) ) ;
#2514 = AXIS2_PLACEMENT_3D ( 'NONE', #3192, #17961, #1240 ) ;
#2515 = CARTESIAN_POINT ( 'NONE',  ( 4.488154563753997905, 12.44456933786999286, 1.490167364050000609 ) ) ;
#2516 = CARTESIAN_POINT ( 'NONE',  ( 2.125811182162558932, 28.98043553802446937, 0.3935857075586116638 ) ) ;
#2517 = CARTESIAN_POINT ( 'NONE',  ( -21.93566186853000133, 8.065990246855999857, 7.630410654556999184 ) ) ;
#2518 = ORIENTED_EDGE ( 'NONE', *, *, #4350, .F. ) ;
#2519 = B_SPLINE_CURVE_WITH_KNOTS ( 'NONE', 3,
 ( #6893, #19859, #4849, #21559, #14288, #6534, #1206, #10420, #14164, #15845 ),
 .UNSPECIFIED., .F., .F.,
 ( 4, 2, 2, 2, 4 ),
 ( 0.000000000000000000, 0.2499999999999942268, 0.3749999999999960032, 0.4999999999999977796, 1.000000000000000000 ),
 .UNSPECIFIED. ) ;
#2520 = FACE_OUTER_BOUND ( 'NONE', #11992, .T. ) ;
#2521 = ORIENTED_EDGE ( 'NONE', *, *, #18719, .F. ) ;
#2522 = DIRECTION ( 'NONE',  ( -1.000000000000000000, 0.000000000000000000, 0.000000000000000000 ) ) ;
#2523 = CARTESIAN_POINT ( 'NONE',  ( 2.400996485352273613, 11.81767763009764316, 4.145245190034037464 ) ) ;
#2524 = CARTESIAN_POINT ( 'NONE',  ( -2.688159063712002084, 13.03541276042999364, 5.879976109452004884 ) ) ;
#2525 = CARTESIAN_POINT ( 'NONE',  ( -1.257898175673276331, 6.893178841067931550, 1.219165795350648285 ) ) ;
#2526 = CARTESIAN_POINT ( 'NONE',  ( 16.62693924930999856, 10.62505432564000074, 1.551621659364999850 ) ) ;
#2527 = EDGE_CURVE ( 'NONE', #12621, #23059, #22959, .T. ) ;
#2528 = CARTESIAN_POINT ( 'NONE',  ( -16.24575980504999606, 10.15426072268999924, 3.750674035441000420 ) ) ;
#2529 = VECTOR ( 'NONE', #15495, 1000.000000000000000 ) ;
#2530 = CARTESIAN_POINT ( 'NONE',  ( 11.61168875731000050, -4.628380041800000733, -7.810153319783999848 ) ) ;
#2531 = CARTESIAN_POINT ( 'NONE',  ( 24.49999999999999645, 0.5123787730663634798, 12.50000000000000000 ) ) ;
#2532 = ORIENTED_EDGE ( 'NONE', *, *, #10996, .F. ) ;
#2533 = FILL_AREA_STYLE ('',( #22630 ) ) ;
#2534 = CARTESIAN_POINT ( 'NONE',  ( -2.519435264877999625, 25.07075108241999928, -0.1759572809729000042 ) ) ;
#2535 = CARTESIAN_POINT ( 'NONE',  ( 13.84544698529813367, -8.681709169862820374, 5.549329201613704576 ) ) ;
#2536 = ORIENTED_EDGE ( 'NONE', *, *, #1522, .T. ) ;
#2537 = CARTESIAN_POINT ( 'NONE',  ( -0.7159621321844995556, 13.80975668258999178, -6.133614306996999943 ) ) ;
#2538 = CARTESIAN_POINT ( 'NONE',  ( -23.97728971654279917, 13.40084515676303312, -1.788539470789224595 ) ) ;
#2539 = CARTESIAN_POINT ( 'NONE',  ( 2.701604807922000084, 30.19703527822999689, -0.4899141053905000653 ) ) ;
#2540 = ADVANCED_FACE ( 'NONE', ( #23055 ), #15665, .T. ) ;
#2541 = CARTESIAN_POINT ( 'NONE',  ( -11.04281598264000053, 15.43375672974000068, 0.000000000000000000 ) ) ;
#2542 = CARTESIAN_POINT ( 'NONE',  ( 18.32283200093110054, 10.42794303851333737, -0.8528220165487894189 ) ) ;
#2543 = DIRECTION ( 'NONE',  ( 0.000000000000000000, 0.000000000000000000, -1.000000000000000000 ) ) ;
#2544 = CARTESIAN_POINT ( 'NONE',  ( 0.000000000000000000, 16.89999999999999858, 0.000000000000000000 ) ) ;
#2545 = FACE_OUTER_BOUND ( 'NONE', #14555, .T. ) ;
#2546 = ORIENTED_EDGE ( 'NONE', *, *, #19568, .F. ) ;
#2547 = CIRCLE ( 'NONE', #18800, 7.100000000000000533 ) ;
#2548 = CYLINDRICAL_SURFACE ( 'NONE', #14997, 7.100000000000000533 ) ;
#2549 = ORIENTED_EDGE ( 'NONE', *, *, #9120, .F. ) ;
#2550 = CARTESIAN_POINT ( 'NONE',  ( -6.042815832213999983, 16.39253418350000047, -0.9999999878869999526 ) ) ;
#2552 = CARTESIAN_POINT ( 'NONE',  ( -2.103837132995996839, 23.84009889363539259, 0.6191421011388187345 ) ) ;
#2551 = CARTESIAN_POINT ( 'NONE',  ( -4.446287379418881969, 12.30056135601858713, 1.928247084751353535 ) ) ;
#2553 = CARTESIAN_POINT ( 'NONE',  ( -3.653528746112522541, 28.20780860099737097, -2.509315635920815524 ) ) ;
#2554 = CARTESIAN_POINT ( 'NONE',  ( 14.77207488446000028, 6.658492172936999687, -8.784828455393000723 ) ) ;
#2555 = CARTESIAN_POINT ( 'NONE',  ( -5.981181950157998806, 15.11060635804999741, -2.632465999322001426 ) ) ;
#2556 = EDGE_CURVE ( 'NONE', #18990, #5263, #11534, .T. ) ;
#2557 = CARTESIAN_POINT ( 'NONE',  ( -2.449293598294692609E-16, 9.100092063578999912, 1.999999999999988676 ) ) ;
#2558 = VERTEX_POINT ( 'NONE', #22301 ) ;
#2559 = VERTEX_POINT ( 'NONE', #18913 ) ;
#2560 = CARTESIAN_POINT ( 'NONE',  ( -14.00000000000000178, -4.872638669815645862, -8.474582696947910776 ) ) ;
#2561 = CARTESIAN_POINT ( 'NONE',  ( 2.817565069457256932, 29.94682129341587284, -2.992080202207098694 ) ) ;
#2562 = DIRECTION ( 'NONE',  ( -0.000000000000000000, 1.000000000000000000, 0.000000000000000000 ) ) ;
#2563 = ORIENTED_EDGE ( 'NONE', *, *, #19487, .F. ) ;
#2564 = CARTESIAN_POINT ( 'NONE',  ( -18.57447842246000036, -9.039081325395999400, -0.2073323074504999919 ) ) ;
#2565 = CARTESIAN_POINT ( 'NONE',  ( 0.000000000000000000, 7.100000000000000533, 0.000000000000000000 ) ) ;
#2566 = AXIS2_PLACEMENT_3D ( 'NONE', #18094, #1502, #16262 ) ;
#2567 = CARTESIAN_POINT ( 'NONE',  ( 6.146311545762546125, 14.15705020831570593, 0.1884214613589945964 ) ) ;
#2568 = CARTESIAN_POINT ( 'NONE',  ( 15.84391418034966215, -10.32692765650489797, -0.7703782186506803464 ) ) ;
#2569 = AXIS2_PLACEMENT_3D ( 'NONE', #11576, #9749, #2008 ) ;
#2570 = CARTESIAN_POINT ( 'NONE',  ( -14.91210445643999982, 9.869058056742000318, 4.894649932895999811 ) ) ;
#2571 = CARTESIAN_POINT ( 'NONE',  ( -2.000000000000000000, 28.00000000000000000, -3.464101615137999968 ) ) ;
#2572 = ADVANCED_FACE ( 'NONE', ( #3789 ), #13104, .F. ) ;
#2573 = CARTESIAN_POINT ( 'NONE',  ( -19.60932161866278278, -9.094709918404200621, 5.216993370950443243 ) ) ;
#2574 = DIRECTION ( 'NONE',  ( 0.000000000000000000, -1.000000000000000000, 0.000000000000000000 ) ) ;
#2575 = CARTESIAN_POINT ( 'NONE',  ( -1.521839280563020536, 29.50435537852937529, 1.532609397753554648 ) ) ;
#2576 = ORIENTED_EDGE ( 'NONE', *, *, #14807, .F. ) ;
#2577 = AXIS2_PLACEMENT_3D ( 'NONE', #8303, #2736, #23301 ) ;
#2578 = CARTESIAN_POINT ( 'NONE',  ( 2.108233021187000400, 25.66491687433000024, -0.7394748174873000401 ) ) ;
#2579 = CARTESIAN_POINT ( 'NONE',  ( -14.31831880116688538, -5.229320062394984703, 8.931164432586227164 ) ) ;
#2580 = CIRCLE ( 'NONE', #18829, 1.750000000000000444 ) ;
#2581 = VERTEX_POINT ( 'NONE', #20502 ) ;
#2582 = DIRECTION ( 'NONE',  ( 1.000000000000000000, 0.000000000000000000, -2.088598344706999779E-09 ) ) ;
#2583 = CARTESIAN_POINT ( 'NONE',  ( 6.626584110769001335, 13.50257275877999064, -0.5067788187794998178 ) ) ;
#2584 = CARTESIAN_POINT ( 'NONE',  ( -19.91867920454665608, 2.403600030157754919, -8.943391512361417384 ) ) ;
#2585 = ADVANCED_FACE ( 'NONE', ( #18788 ), #15261, .F. ) ;
#2586 = CARTESIAN_POINT ( 'NONE',  ( 13.06406392131000160, -4.637122060904999898, 8.435305548789999719 ) ) ;
#2587 = EDGE_CURVE ( 'NONE', #5160, #16051, #19089, .T. ) ;
#2588 = ORIENTED_EDGE ( 'NONE', *, *, #16504, .T. ) ;
#2589 = CARTESIAN_POINT ( 'NONE',  ( 18.45420603379666247, -7.704153391283862007, 5.039298146494758157 ) ) ;
#2590 = CARTESIAN_POINT ( 'NONE',  ( 0.3272492347489343589, 26.98333333333333428, -2.500000000000000444 ) ) ;
#2591 = CARTESIAN_POINT ( 'NONE',  ( -7.500000000000000000, 22.00000000000000000, 1.000000000000000000 ) ) ;
#2592 = EDGE_LOOP ( 'NONE', ( #52, #23233, #244 ) ) ;
#2593 = DIRECTION ( 'NONE',  ( 0.000000000000000000, -1.000000000000000000, 0.000000000000000000 ) ) ;
#2594 = CARTESIAN_POINT ( 'NONE',  ( 12.52688711657000020, 7.716878364870000340, 11.63397459621999985 ) ) ;
#2595 = CARTESIAN_POINT ( 'NONE',  ( 4.813190031656002787, 12.64298052023998586, 0.2515842787466999186 ) ) ;
#2596 = DIRECTION ( 'NONE',  ( 0.000000000000000000, 1.000000000000000000, 0.000000000000000000 ) ) ;
#2597 = CARTESIAN_POINT ( 'NONE',  ( 17.66152877879916261, -10.36100141562122268, -0.9108117703243313601 ) ) ;
#2598 = AXIS2_PLACEMENT_3D ( 'NONE', #11856, #17802, #4840 ) ;
#2599 = DIRECTION ( 'NONE',  ( 0.000000000000000000, -1.000000000000000000, 0.000000000000000000 ) ) ;
#2600 = CARTESIAN_POINT ( 'NONE',  ( 0.000000000000000000, 18.00000000000000000, 0.000000000000000000 ) ) ;
#2602 = ADVANCED_FACE ( 'NONE', ( #3668 ), #16397, .T. ) ;
#2601 = CARTESIAN_POINT ( 'NONE',  ( 22.10687615272999906, 7.216905606319000022, 8.629172509395999668 ) ) ;
#2603 = AXIS2_PLACEMENT_3D ( 'NONE', #5656, #9656, #20438 ) ;
#2604 = EDGE_CURVE ( 'NONE', #18376, #10732, #23071, .T. ) ;
#2605 = LINE ( 'NONE', #22937, #14697 ) ;
#2606 = CARTESIAN_POINT ( 'NONE',  ( 5.801373033572341242, 14.45988999510258388, 1.973196774158483935 ) ) ;
#2607 = FACE_OUTER_BOUND ( 'NONE', #7377, .T. ) ;
#2608 = CIRCLE ( 'NONE', #1465, 7.142857142857000241 ) ;
#2609 = CARTESIAN_POINT ( 'NONE',  ( -2.159859212911454662, 30.20451953216726082, 0.01416237932336155032 ) ) ;
#2610 = ORIENTED_EDGE ( 'NONE', *, *, #22703, .T. ) ;
#2611 = CARTESIAN_POINT ( 'NONE',  ( -16.56112077250667269, -9.096272712312636344, 1.190572366013356698 ) ) ;
#2612 = CARTESIAN_POINT ( 'NONE',  ( 18.35893224774000032, 0.1033670869143000076, 9.766723590596999571 ) ) ;
#2613 = CARTESIAN_POINT ( 'NONE',  ( 0.8106507644720812866, 12.82603987343919094, -6.620134064058884604 ) ) ;
#2614 = DIRECTION ( 'NONE',  ( 0.000000000000000000, 0.000000000000000000, 1.000000000000000000 ) ) ;
#2615 = CARTESIAN_POINT ( 'NONE',  ( -20.91203816579346508, -8.901941407118242111, -5.604029123285282132 ) ) ;
#2616 = LINE ( 'NONE', #8311, #4226 ) ;
#2617 = AXIS2_PLACEMENT_3D ( 'NONE', #21150, #7203, #8679 ) ;
#2618 = B_SPLINE_CURVE_WITH_KNOTS ( 'NONE', 3,
 ( #8427, #19448, #15910, #23300, #17876, #6715, #21502, #1277, #8662, #21628 ),
 .UNSPECIFIED., .F., .F.,
 ( 4, 1, 1, 2, 2, 4 ),
 ( 0.000000000000000000, 0.2499999999999986677, 0.3749999999999980016, 0.4374999999999982236, 0.4999999999999984457, 1.000000000000000000 ),
 .UNSPECIFIED. ) ;
#2619 = AXIS2_PLACEMENT_3D ( 'NONE', #12169, #23045, #1147 ) ;
#2620 = CARTESIAN_POINT ( 'NONE',  ( -6.199443458293737663, 26.48693030808626503, 1.100246419409809828 ) ) ;
#2621 = VERTEX_POINT ( 'NONE', #18564 ) ;
#2622 = CARTESIAN_POINT ( 'NONE',  ( -19.13574525531997494, -9.517642123610587035, -4.380541451279561294 ) ) ;
#2623 = DIRECTION ( 'NONE',  ( 1.000000000000000000, 0.000000000000000000, 0.000000000000000000 ) ) ;
#2624 = CARTESIAN_POINT ( 'NONE',  ( 2.999999998122344191, 21.89999999999998437, 6.187284373140837446E-09 ) ) ;
#2625 = DIRECTION ( 'NONE',  ( 0.000000000000000000, -0.03830820919371688560, 0.9992659711550128110 ) ) ;
#2626 = CARTESIAN_POINT ( 'NONE',  ( 0.000000000000000000, 22.00000000000000000, 0.000000000000000000 ) ) ;
#2627 = ORIENTED_EDGE ( 'NONE', *, *, #18310, .T. ) ;
#2628 = CARTESIAN_POINT ( 'NONE',  ( 16.84508103379666721, -9.103559692274046711, -1.191526229459736408 ) ) ;
#2629 = CARTESIAN_POINT ( 'NONE',  ( 13.55568924931000119, -5.133899498893999436, 9.338903284905999413 ) ) ;
#2630 = CARTESIAN_POINT ( 'NONE',  ( -24.05893800299999796, 10.23807085788999949, -4.603936266037999658 ) ) ;
#2631 = CARTESIAN_POINT ( 'NONE',  ( 3.000000000000000000, 22.00000000000000000, 0.000000000000000000 ) ) ;
#2632 = DIRECTION ( 'NONE',  ( 0.000000000000000000, 0.000000000000000000, 1.000000000000000000 ) ) ;
#2633 = CARTESIAN_POINT ( 'NONE',  ( 15.39619494526000132, 10.26707030725000003, -0.2369671920225999984 ) ) ;
#2634 = CARTESIAN_POINT ( 'NONE',  ( -4.000000000000000888, 26.42936170367563520, -1.090349405812125916 ) ) ;
#2635 = AXIS2_PLACEMENT_3D ( 'NONE', #11556, #20633, #272 ) ;
#2636 = CARTESIAN_POINT ( 'NONE',  ( 2.500000000000001776, 27.01753006952333180, 0.3272492347489266429 ) ) ;
#2637 = CARTESIAN_POINT ( 'NONE',  ( 22.35490775615000203, -3.982320853531000182, -8.877099480003998622 ) ) ;
#2638 = B_SPLINE_SURFACE_WITH_KNOTS ( 'NONE', 3, 3, ( 
 ( #6861, #9248, #4701, #14012 ),
 ( #19717, #12447, #19831, #15930 ),
 ( #19591, #6738, #14132, #16625 ),
 ( #14254, #21289, #1048, #6504 ) ),
 .UNSPECIFIED., .F., .F., .F.,
 ( 4, 4 ),
 ( 4, 4 ),
 ( -0.09148521614644000710, 0.2147869640759000054 ),
 ( 0.9473429275995000065, 1.001032491615999831 ),
 .UNSPECIFIED. ) ;
#2639 = CARTESIAN_POINT ( 'NONE',  ( 3.064125534931650296, 29.91068681084919234, 2.849728451093327397 ) ) ;
#2640 = ORIENTED_EDGE ( 'NONE', *, *, #1705, .F. ) ;
#2641 = CARTESIAN_POINT ( 'NONE',  ( 18.64355344916001300, -1.808540911500012838, 9.835923363989143908 ) ) ;
#2642 = CARTESIAN_POINT ( 'NONE',  ( -1.733846816785000078, 27.84456776952000112, -2.030073792688000367 ) ) ;
#2643 = CARTESIAN_POINT ( 'NONE',  ( -0.1141952544650000068, 11.49080619599998876, 4.810811492839003556 ) ) ;
#2644 = CARTESIAN_POINT ( 'NONE',  ( 2.155020325414803040, 28.99531748523413910, 0.1450810396632776778 ) ) ;
#2645 = AXIS2_PLACEMENT_3D ( 'NONE', #13023, #3706, #11227 ) ;
#2646 = PRODUCT_DEFINITION ( 'UNKNOWN', '', #13660, #8910 ) ;
#2647 = CARTESIAN_POINT ( 'NONE',  ( -20.11819481384999975, 10.67730650337000142, 2.861074714015000353 ) ) ;
#2648 = CARTESIAN_POINT ( 'NONE',  ( 0.000000000000000000, -13.00000000000000000, 0.000000000000000000 ) ) ;
#2649 = CIRCLE ( 'NONE', #9995, 10.59999999999999964 ) ;
#2650 = ORIENTED_EDGE ( 'NONE', *, *, #14392, .T. ) ;
#2651 = CARTESIAN_POINT ( 'NONE',  ( 15.14445603379664895, -7.916481873543318670, -4.562629533669052329 ) ) ;
#2652 = CARTESIAN_POINT ( 'NONE',  ( -19.78832264027077059, -9.441231315352206721, 3.364601191696911631 ) ) ;
#2653 = CARTESIAN_POINT ( 'NONE',  ( 3.118723778390000589, 14.26802845704001754, 5.330537660070998385 ) ) ;
#2654 = CARTESIAN_POINT ( 'NONE',  ( -1.507771686977886771, 6.943202342706179309, 0.8987492179439539042 ) ) ;
#2655 = PLANE ( 'NONE',  #4969 ) ;
#2656 = CARTESIAN_POINT ( 'NONE',  ( -6.250000000000000000, 15.73203524433000311, -1.185075242810999852 ) ) ;
#2657 = CARTESIAN_POINT ( 'NONE',  ( 17.64450125731000085, 9.220888413547999818, -0.5479559280035000146 ) ) ;
#2658 = DIRECTION ( 'NONE',  ( 0.000000000000000000, 1.000000000000000000, 0.000000000000000000 ) ) ;
#2659 = VECTOR ( 'NONE', #23963, 1000.000000000000000 ) ;
#2660 = ORIENTED_EDGE ( 'NONE', *, *, #12790, .F. ) ;
#2661 = CARTESIAN_POINT ( 'NONE',  ( 20.02908892782178540, 9.445433025424275542, -4.628470371599332722 ) ) ;
#2662 = CARTESIAN_POINT ( 'NONE',  ( 2.483627104365000005, 30.80612887107999853, 1.118432463241999963 ) ) ;
#2663 = CARTESIAN_POINT ( 'NONE',  ( -1.962698410735999488, 24.36629882400999847, 1.589443273402000090 ) ) ;
#2664 = CIRCLE ( 'NONE', #5003, 12.34057940292999866 ) ;
#2665 = CARTESIAN_POINT ( 'NONE',  ( 3.425434194794530818, 14.25881501014746888, -5.078536901545239068 ) ) ;
#2666 = AXIS2_PLACEMENT_3D ( 'NONE', #9687, #584, #17068 ) ;
#2667 = ORIENTED_EDGE ( 'NONE', *, *, #7066, .F. ) ;
#2668 = CARTESIAN_POINT ( 'NONE',  ( 5.752440845993000096, 13.85430232992000299, -4.060540161502004253 ) ) ;
#2669 = CARTESIAN_POINT ( 'NONE',  ( 20.34417738779000473, 9.978297411703000108, -5.088582451532000839 ) ) ;
#2670 = CARTESIAN_POINT ( 'NONE',  ( 0.2870741741112000089, 28.76085756624999945, -2.730617656758999701 ) ) ;
#2671 = CARTESIAN_POINT ( 'NONE',  ( 11.70388046502320201, -4.051054454411410433, 12.49994163046800288 ) ) ;
#2672 = DIRECTION ( 'NONE',  ( -0.9996708941621509359, 0.02565352539214875091, 1.648348900435920369E-14 ) ) ;
#2673 = CARTESIAN_POINT ( 'NONE',  ( 0.000000000000000000, 13.00000000000000000, 0.000000000000000000 ) ) ;
#2674 = AXIS2_PLACEMENT_3D ( 'NONE', #5106, #21695, #3048 ) ;
#2675 = CARTESIAN_POINT ( 'NONE',  ( -18.63376253787999914, -9.149460784975000038, 0.000000000000000000 ) ) ;
#2676 = EDGE_CURVE ( 'NONE', #20521, #6064, #21068, .T. ) ;
#2677 = CARTESIAN_POINT ( 'NONE',  ( 1.259047450927247569, 29.56753006952333607, -2.184465970885645536 ) ) ;
#2678 = ORIENTED_EDGE ( 'NONE', *, *, #5292, .F. ) ;
#2679 = CARTESIAN_POINT ( 'NONE',  ( 2.309807618587000011, 30.69019238141000017, -7.292675330123999428E-08 ) ) ;
#2680 = CARTESIAN_POINT ( 'NONE',  ( 0.7867367962552690441, 24.50000000000000000, -2.267387309971103271 ) ) ;
#2681 = VERTEX_POINT ( 'NONE', #13452 ) ;
#2682 = TOROIDAL_SURFACE ( 'NONE', #8888, 13.91261088316000105, 1.521145846583000116 ) ;
#2683 = FACE_OUTER_BOUND ( 'NONE', #21589, .T. ) ;
#2684 = CARTESIAN_POINT ( 'NONE',  ( 2.184465970885652641, 28.56753006952332186, 1.259047450927233580 ) ) ;
#2685 = CARTESIAN_POINT ( 'NONE',  ( 3.958466783697788038, 13.32814196193950984, 5.540440575617210150 ) ) ;
#2686 = AXIS2_PLACEMENT_3D ( 'NONE', #21442, #4856, #12121 ) ;
#2687 = CYLINDRICAL_SURFACE ( 'NONE', #18834, 7.000000000000000000 ) ;
#2688 = CARTESIAN_POINT ( 'NONE',  ( 7.446152422707000618, 28.20096189432300093, -6.000000000000000000 ) ) ;
#2689 = VECTOR ( 'NONE', #3314, 1000.000000000000114 ) ;
#2690 = CARTESIAN_POINT ( 'NONE',  ( -1.626917502017769523, 26.50000000000000355, 1.884902535258590195 ) ) ;
#2691 = ADVANCED_FACE ( 'NONE', ( #11179, #1969 ), #9352, .F. ) ;
#2692 = EDGE_LOOP ( 'NONE', ( #19556, #23252 ) ) ;
#2693 = VERTEX_POINT ( 'NONE', #251 ) ;
#2694 = CARTESIAN_POINT ( 'NONE',  ( 7.124999988904000325, 14.37502327612999942, -5.687882594960999921E-06 ) ) ;
#2695 = AXIS2_PLACEMENT_3D ( 'NONE', #398, #632, #5740 ) ;
#2696 = CARTESIAN_POINT ( 'NONE',  ( -1.888459278277104156E-11, 26.49469377355791977, -2.394693773557865057 ) ) ;
#2697 = CARTESIAN_POINT ( 'NONE',  ( -6.517755120876246089, 15.19342473677416727, -2.753401504715822679 ) ) ;
#2698 = ORIENTED_EDGE ( 'NONE', *, *, #180, .F. ) ;
#2699 = DIRECTION ( 'NONE',  ( 0.000000000000000000, -1.000000000000000000, 0.000000000000000000 ) ) ;
#2700 = DIRECTION ( 'NONE',  ( 0.000000000000000000, 0.000000000000000000, -1.000000000000000000 ) ) ;
#2701 = CARTESIAN_POINT ( 'NONE',  ( 15.06374514717642477, 9.021709532834009337, 5.042244869155494413 ) ) ;
#2702 = CARTESIAN_POINT ( 'NONE',  ( -14.18945119630999940, -10.82201390087000092, 1.947477006705999880 ) ) ;
#2703 = AXIS2_PLACEMENT_3D ( 'NONE', #11095, #9280, #10977 ) ;
#2704 = DIRECTION ( 'NONE',  ( -1.000000000000000000, 0.000000000000000000, 0.000000000000000000 ) ) ;
#2705 = CARTESIAN_POINT ( 'NONE',  ( -19.81520262463921611, -3.472309042968596771, 9.897195304290566042 ) ) ;
#2706 = CARTESIAN_POINT ( 'NONE',  ( -14.05208405859999843, -9.143870435873997948, 6.637879840603000403 ) ) ;
#2707 = EDGE_CURVE ( 'NONE', #19991, #903, #9590, .T. ) ;
#2708 = CARTESIAN_POINT ( 'NONE',  ( -2.063376835572392487, 29.44210936106684429, 0.6381193817384768208 ) ) ;
#2709 = VERTEX_POINT ( 'NONE', #5834 ) ;
#2710 = CARTESIAN_POINT ( 'NONE',  ( 2.243357345374999756, 25.64165095250000093, -0.3542371386884999862 ) ) ;
#2711 = CARTESIAN_POINT ( 'NONE',  ( -17.27011453369921057, -2.826153282971739511, -10.04434318468920573 ) ) ;
#2712 = AXIS2_PLACEMENT_3D ( 'NONE', #14859, #2268, #321 ) ;
#2713 = ORIENTED_EDGE ( 'NONE', *, *, #2867, .F. ) ;
#2714 = CARTESIAN_POINT ( 'NONE',  ( -23.75391236596000155, 7.467096437641000506, -11.77818625913999817 ) ) ;
#2715 = CARTESIAN_POINT ( 'NONE',  ( 5.625313445317996930, 13.77071113236998379, -3.543115536436998170 ) ) ;
#2716 = CARTESIAN_POINT ( 'NONE',  ( 12.00000000000000000, -3.611861960331876897, -8.220758729215566163 ) ) ;
#2717 = FACE_OUTER_BOUND ( 'NONE', #17296, .T. ) ;
#2718 = EDGE_CURVE ( 'NONE', #22144, #6663, #13217, .T. ) ;
#2719 = CARTESIAN_POINT ( 'NONE',  ( 12.29625142131000004, 8.002767958507000401, -5.312704480003000995 ) ) ;
#2720 = ORIENTED_EDGE ( 'NONE', *, *, #12795, .F. ) ;
#2721 = DIRECTION ( 'NONE',  ( 0.000000000000000000, 1.000000000000000000, 0.000000000000000000 ) ) ;
#2722 = DIRECTION ( 'NONE',  ( 1.000000000000000000, 0.000000000000000000, 0.000000000000000000 ) ) ;
#2723 = CARTESIAN_POINT ( 'NONE',  ( 2.164939593608601776, 24.49999999999984368, -3.368873696368142490 ) ) ;
#2724 = ORIENTED_EDGE ( 'NONE', *, *, #14550, .T. ) ;
#2725 = DIRECTION ( 'NONE',  ( 0.000000000000000000, 1.000000000000000000, 0.000000000000000000 ) ) ;
#2726 = CARTESIAN_POINT ( 'NONE',  ( -23.74465998031000069, -13.93375672974000068, -0.8660254037843999608 ) ) ;
#2727 = CARTESIAN_POINT ( 'NONE',  ( 24.26478934590349468, -0.8345397459580851107, 10.59477908038717686 ) ) ;
#2728 = CARTESIAN_POINT ( 'NONE',  ( -12.48243343204000055, 6.965111533508000718, -5.686492047758000545 ) ) ;
#2729 = CARTESIAN_POINT ( 'NONE',  ( 18.06179173045719821, -1.003953116814803481, -10.36291011014150065 ) ) ;
#2730 = EDGE_CURVE ( 'NONE', #16405, #2468, #1322, .T. ) ;
#2731 = CARTESIAN_POINT ( 'NONE',  ( 12.00000000000000178, -5.648153558507000405, -7.896738249884089456 ) ) ;
#2732 = CARTESIAN_POINT ( 'NONE',  ( -14.37382047448982192, -8.632461983038391296, 10.04764370666022444 ) ) ;
#2733 = CARTESIAN_POINT ( 'NONE',  ( 18.80303081932999731, -4.612880036109999082, 10.15984863128999827 ) ) ;
#2734 = DIRECTION ( 'NONE',  ( -1.000000000000000000, 0.000000000000000000, 0.000000000000000000 ) ) ;
#2735 = CARTESIAN_POINT ( 'NONE',  ( -3.998638495880459498, 13.85419791046053994, -4.853578403047964507 ) ) ;
#2736 = DIRECTION ( 'NONE',  ( 0.000000000000000000, 1.000000000000000000, 0.000000000000000000 ) ) ;
#2737 = EDGE_CURVE ( 'NONE', #10311, #22357, #3267, .T. ) ;
#2738 = CARTESIAN_POINT ( 'NONE',  ( -1.850862556816144755, 30.13458432399187004, -1.117312800271740736 ) ) ;
#2739 = ORIENTED_EDGE ( 'NONE', *, *, #6904, .T. ) ;
#2740 = EDGE_CURVE ( 'NONE', #23570, #10530, #10318, .T. ) ;
#2741 = CARTESIAN_POINT ( 'NONE',  ( -16.93903743917333315, -1.192095737878614781, 9.105970798813979528 ) ) ;
#2742 = CARTESIAN_POINT ( 'NONE',  ( 18.87426807056999678, -10.06611063169999909, -2.115216155665999853 ) ) ;
#2743 = CARTESIAN_POINT ( 'NONE',  ( 3.177045621698409317, 13.14387179043593079, -5.964232631809895935 ) ) ;
#2744 = CARTESIAN_POINT ( 'NONE',  ( -0.6543697108981929578, 27.60086340285666751, 2.434931691670791487 ) ) ;
#2745 = CARTESIAN_POINT ( 'NONE',  ( 1.640193969998194001, 24.74015355458762144, 1.405240085690787843 ) ) ;
#2746 = CARTESIAN_POINT ( 'NONE',  ( -24.41904027017961454, -11.84953030590303591, -4.475986625628626925 ) ) ;
#2747 = CARTESIAN_POINT ( 'NONE',  ( -4.282263979383000851, 12.27659869337001552, -2.483328958996001479 ) ) ;
#2748 = VERTEX_POINT ( 'NONE', #978 ) ;
#2749 = CARTESIAN_POINT ( 'NONE',  ( -18.74498793411180131, 2.216523406432389098, -10.23078730626788158 ) ) ;
#2750 = EDGE_CURVE ( 'NONE', #9910, #6464, #5568, .T. ) ;
#2751 = DIRECTION ( 'NONE',  ( 0.000000000000000000, -1.000000000000000000, 0.000000000000000000 ) ) ;
#2752 = CARTESIAN_POINT ( 'NONE',  ( -1.960246057973615619, 27.56955929831042695, -0.9957143590686239332 ) ) ;
#2753 = CIRCLE ( 'NONE', #13178, 4.000000000000000000 ) ;
#2754 = APPLICATION_PROTOCOL_DEFINITION ( 'draft international standard', 'automotive_design', 1998, #1066 ) ;
#2755 = EDGE_LOOP ( 'NONE', ( #1706, #2222, #5122, #12171, #3062 ) ) ;
#2756 = ORIENTED_EDGE ( 'NONE', *, *, #9269, .T. ) ;
#2757 = CARTESIAN_POINT ( 'NONE',  ( 17.63870603379666946, 8.886405729592773639, -2.388285526542218040 ) ) ;
#2758 = CARTESIAN_POINT ( 'NONE',  ( 19.00350174931000069, -5.312632942934000013, 9.204603991398000673 ) ) ;
#2759 = CARTESIAN_POINT ( 'NONE',  ( -14.02955537940998809, 6.411209705375615187, -6.427717830503866026 ) ) ;
#2760 = CARTESIAN_POINT ( 'NONE',  ( -17.25423626710000136, 5.368550673722999989, -9.432097563122999517 ) ) ;
#2761 = CARTESIAN_POINT ( 'NONE',  ( -6.044422725124001694, 15.62653472375999542, 1.260791734048000379 ) ) ;
#2762 = CARTESIAN_POINT ( 'NONE',  ( 14.98994494525999954, 1.437436215449000132, -10.15727603318000050 ) ) ;
#2763 = CARTESIAN_POINT ( 'NONE',  ( -4.000000000000000888, 26.46241504948188705, -0.8002143650531428065 ) ) ;
#2764 = DIRECTION ( 'NONE',  ( 0.000000000000000000, -1.000000000000000000, 0.000000000000000000 ) ) ;
#2765 = CARTESIAN_POINT ( 'NONE',  ( 24.41097397878344921, 9.853094029288689271, 1.034144647742462508 ) ) ;
#2766 = VERTEX_POINT ( 'NONE', #20970 ) ;
#2767 = CARTESIAN_POINT ( 'NONE',  ( 2.541770361367480913, 14.00639520368903312, 5.573038258459499517 ) ) ;
#2768 = CARTESIAN_POINT ( 'NONE',  ( -0.7744564004552000336, 28.91706776952000268, 2.554499528901000183 ) ) ;
#2769 = CARTESIAN_POINT ( 'NONE',  ( -4.607457922294000419, 12.49060724118000110, 1.057233348562000685 ) ) ;
#2770 = CARTESIAN_POINT ( 'NONE',  ( 3.268181200173221335, 26.37490599056235752, 2.731916857836432566 ) ) ;
#2771 = CARTESIAN_POINT ( 'NONE',  ( -20.24435346183999940, 7.375945635487999752, 8.237836394566999232 ) ) ;
#2772 = DIRECTION ( 'NONE',  ( 0.000000000000000000, 1.000000000000000000, 0.000000000000000000 ) ) ;
#2773 = B_SPLINE_CURVE_WITH_KNOTS ( 'NONE', 3,
 ( #15195, #8189, #541, #18961, #9758, #5769, #16898, #7946, #3958, #4311 ),
 .UNSPECIFIED., .F., .F.,
 ( 4, 2, 2, 2, 4 ),
 ( 0.000000000000000000, 0.2500000000000000000, 0.5000000000000000000, 0.7500000000000000000, 1.000000000000000000 ),
 .UNSPECIFIED. ) ;
#2774 = ORIENTED_EDGE ( 'NONE', *, *, #1568, .F. ) ;
#2775 = FACE_OUTER_BOUND ( 'NONE', #11419, .T. ) ;
#2776 = LINE ( 'NONE', #824, #20916 ) ;
#2777 = ADVANCED_FACE ( 'NONE', ( #6557 ), #4028, .T. ) ;
#2778 = CARTESIAN_POINT ( 'NONE',  ( -4.005628047234999656, 13.41105388907000417, 5.056273175647006290 ) ) ;
#2779 = EDGE_CURVE ( 'NONE', #14211, #3898, #9531, .T. ) ;
#2780 = DIRECTION ( 'NONE',  ( 0.000000000000000000, 1.000000000000000000, 0.000000000000000000 ) ) ;
#2781 = FACE_OUTER_BOUND ( 'NONE', #22912, .T. ) ;
#2782 = CARTESIAN_POINT ( 'NONE',  ( -12.43257971169000164, 9.053737661458001185, -12.66555795296999953 ) ) ;
#2783 = CARTESIAN_POINT ( 'NONE',  ( -8.000000000000000000, 1.322618543078999814E-14, 0.000000000000000000 ) ) ;
#2784 = CARTESIAN_POINT ( 'NONE',  ( 17.86387625731000028, 7.066414026761999700, 5.957971218261000956 ) ) ;
#2785 = CARTESIAN_POINT ( 'NONE',  ( -2.184465970885641539, 27.26666666666667282, 1.259047450927253120 ) ) ;
#2786 = CIRCLE ( 'NONE', #16311, 1.000000000000000222 ) ;
#2787 = EDGE_LOOP ( 'NONE', ( #19107, #22750, #17271, #10372 ) ) ;
#2788 = CARTESIAN_POINT ( 'NONE',  ( -22.00241225129201794, -9.233902645863798497, 1.209007217019692604 ) ) ;
#2789 = CARTESIAN_POINT ( 'NONE',  ( 1.487891794119999833, 30.63451452002999886, 2.049709317120999685 ) ) ;
#2790 = B_SPLINE_CURVE_WITH_KNOTS ( 'NONE', 3,
 ( #8895, #8768, #18095, #1618, #9117, #7063, #16376, #16131, #14447, #5254, #16491, #23880, #12638, #21610, #20026, #3444, #23533, #9006 ),
 .UNSPECIFIED., .F., .F.,
 ( 4, 2, 2, 2, 2, 2, 2, 2, 4 ),
 ( 0.000000000000000000, 0.1250000000000000000, 0.2500000000000000000, 0.3750000000000000555, 0.5000000000000000000, 0.6250000000000000000, 0.7500000000000000000, 0.8750000000000000000, 1.000000000000000000 ),
 .UNSPECIFIED. ) ;
#2791 = CARTESIAN_POINT ( 'NONE',  ( -1.627763130269000103, 23.49237082063000059, 2.174264886728999979 ) ) ;
#2792 = CARTESIAN_POINT ( 'NONE',  ( 3.099532833261116949, 14.15752231852028231, -5.282866363571895540 ) ) ;
#2793 = ORIENTED_EDGE ( 'NONE', *, *, #5676, .T. ) ;
#2794 = CARTESIAN_POINT ( 'NONE',  ( 5.704330172568996105, 13.83477387354001031, -4.128797533092996019 ) ) ;
#2795 = FILL_AREA_STYLE ('',( #22995 ) ) ;
#2796 = B_SPLINE_SURFACE_WITH_KNOTS ( 'NONE', 3, 3, ( 
 ( #1919, #10782, #18174, #23720, #14403, #22141, #14858, #7127, #22247, #14516, #21909, #3514, #18739, #15459, #4328, #18627, #13640, #6137, #9540, #13282, #14973, #684, #15210, #7962, #2149, #20681, #6257, #18861, #2034, #11719, #11486, #2267, #16917, #17041, #320 ),
 ( #9660, #2506, #7595, #7726, #19094, #22371, #5896, #4090, #439, #5786, #16796, #13169, #9424, #22723, #7841, #202, #9895, #22607, #15091, #22487, #20559, #6016, #13401, #20802, #3857, #11249, #4211, #556, #3973, #20924, #11366, #11605, #13526, #18976, #2385 ),
 ( #9775, #17161, #15334, #17284, #8091, #22844, #15820, #15935, #17783, #19355, #19721, #21163, #23329, #19596, #11966, #10391, #16057, #21530, #14138, #12090, #1182, #4946, #2633, #6742, #2762, #3134, #3006, #4822, #8208, #8453, #15575, #11840, #19474, #21293, #19221 ),
 ( #12330, #21406, #17653, #10518, #1304, #4705, #13761, #2882, #23452, #17901, #23211, #8693, #6866, #21036, #4451, #10029, #10265, #10146, #17414, #809, #1052, #22963, #6378, #4574, #17532, #6627, #926, #8326, #8575, #15691, #23082, #6506, #14016, #13890, #12207 ) ),
 .UNSPECIFIED., .F., .F., .F.,
 ( 4, 4 ),
 ( 4, 1, 1, 1, 1, 1, 1, 1, 1, 1, 1, 1, 1, 1, 1, 1, 1, 1, 1, 1, 1, 1, 1, 1, 1, 1, 1, 1, 1, 1, 1, 1, 4 ),
 ( -0.08331297109794000288, 1.083312971098000066 ),
 ( -0.01851851851851999894, 0.01157407407407000030, 0.04166666666667000196, 0.07175925925925999427, 0.1018518518519000021, 0.1319444444444000109, 0.1620370370369999813, 0.1921296296295999795, 0.2222222222222000054, 0.2523148148148000036, 0.2824074074074000018, 0.3125000000000000000, 0.3425925925925999982, 0.3726851851851999964, 0.4027777777777999946, 0.4328703703703999928, 0.4629629629629999910, 0.4930555555555999891, 0.5231481481480999562, 0.5532407407406999544, 0.5833333333333000637, 0.6134259259259000618, 0.6435185185185000600, 0.6736111111111000582, 0.7037037037036999454, 0.7337962962962999436, 0.7638888888888999418, 0.7939814814814999400, 0.8240740740740999382, 0.8541666666667000474, 0.8842592592593000456, 0.9143518518519000438, 0.9444444444444000109 ),
 .UNSPECIFIED. ) ;
#2797 = CARTESIAN_POINT ( 'NONE',  ( -1.330185344530000036, 29.90979973582999918, 2.401934960883000070 ) ) ;
#2798 = CARTESIAN_POINT ( 'NONE',  ( -12.50000000000000000, 6.868132469527897577, -5.843449823281533284 ) ) ;
#2799 = CARTESIAN_POINT ( 'NONE',  ( 14.53153308584223247, 8.264717062064972808, -6.255766661236222603 ) ) ;
#2800 = CARTESIAN_POINT ( 'NONE',  ( -8.250000000000000000, 18.50000000000000000, 0.000000000000000000 ) ) ;
#2801 = AXIS2_PLACEMENT_3D ( 'NONE', #22276, #7504, #4242 ) ;
#2802 = LINE ( 'NONE', #10183, #10804 ) ;
#2803 = CARTESIAN_POINT ( 'NONE',  ( 20.05737270046332910, -2.404297061055042040, 8.946955187238454954 ) ) ;
#2804 = ORIENTED_EDGE ( 'NONE', *, *, #12744, .T. ) ;
#2805 = CARTESIAN_POINT ( 'NONE',  ( 19.19268716888089443, -6.541906309961956545, 8.200137938995508691 ) ) ;
#2806 = CARTESIAN_POINT ( 'NONE',  ( 1.626104829127729801, 24.49999999999998224, -1.886740530527200255 ) ) ;
#2807 = ORIENTED_EDGE ( 'NONE', *, *, #2676, .T. ) ;
#2808 = CARTESIAN_POINT ( 'NONE',  ( -2.569316494495999859, 25.61518446159000106, -0.9436992233395999907 ) ) ;
#2809 = CARTESIAN_POINT ( 'NONE',  ( 66.60588651278291650, 37.01856778792605240, -1.000000000000000000 ) ) ;
#2810 = FACE_OUTER_BOUND ( 'NONE', #20935, .T. ) ;
#2811 = CIRCLE ( 'NONE', #7827, 12.50000000000000000 ) ;
#2812 = CARTESIAN_POINT ( 'NONE',  ( 1.699999999999999956, 10.36668268731399856, -1.053571508039081506 ) ) ;
#2813 = CARTESIAN_POINT ( 'NONE',  ( -5.384399873003000714, 15.53476682087999805, -2.763068870761999030 ) ) ;
#2814 = CARTESIAN_POINT ( 'NONE',  ( 24.38510397947347741, -2.890284505278647664, -12.49999999999999822 ) ) ;
#2815 = ORIENTED_EDGE ( 'NONE', *, *, #13967, .T. ) ;
#2816 = ORIENTED_EDGE ( 'NONE', *, *, #7137, .T. ) ;
#2817 = CARTESIAN_POINT ( 'NONE',  ( -2.500000000000000000, 29.83419673618999823, 0.000000000000000000 ) ) ;
#2818 = CARTESIAN_POINT ( 'NONE',  ( 3.304996520289661177, 29.87418302490023692, -2.710661522857509276 ) ) ;
#2819 = CARTESIAN_POINT ( 'NONE',  ( 6.696152422707000618, 29.50000000000000000, 6.000000000000000000 ) ) ;
#2820 = ADVANCED_FACE ( 'NONE', ( #17585 ), #9827, .F. ) ;
#2821 = VERTEX_POINT ( 'NONE', #17210 ) ;
#2822 = CARTESIAN_POINT ( 'NONE',  ( 1.740781276729051363, 12.98239425167962935, -1.065112122026150798 ) ) ;
#2823 = CARTESIAN_POINT ( 'NONE',  ( 20.68008333333332160, 2.408479787571709441, -8.962519253214404458 ) ) ;
#2824 = CARTESIAN_POINT ( 'NONE',  ( 14.91301520687590099, 10.33462043395056007, -0.1764324625305463967 ) ) ;
#2825 = CARTESIAN_POINT ( 'NONE',  ( -15.12680948961000027, 7.749013830361000110, -7.838259309650000617 ) ) ;
#2826 = CARTESIAN_POINT ( 'NONE',  ( 2.394884942776999814, 23.89488494277999919, 0.000000000000000000 ) ) ;
#2827 = CARTESIAN_POINT ( 'NONE',  ( -21.51372092398854363, -7.149116854185205483, 7.905589411838503722 ) ) ;
#2828 = CARTESIAN_POINT ( 'NONE',  ( -3.843096720568998315, 12.21397984018998351, -2.758463352735002427 ) ) ;
#2829 = CONICAL_SURFACE ( 'NONE', #16351, 9.161549281532000322, 0.02565634000431304615 ) ;
#2830 = CARTESIAN_POINT ( 'NONE',  ( 0.000000000000000000, 7.100000000000000533, 0.000000000000000000 ) ) ;
#2831 = CARTESIAN_POINT ( 'NONE',  ( -1.845878792324959550, 29.47323799381988962, 1.121740158063918358 ) ) ;
#2832 = VERTEX_POINT ( 'NONE', #854 ) ;
#2833 = CARTESIAN_POINT ( 'NONE',  ( -0.7886471129774000888, 24.23563927490999603, -2.038663358203999909 ) ) ;
#2834 = CARTESIAN_POINT ( 'NONE',  ( -14.81028475658608912, 9.567064880699621909, 4.004655637193650364 ) ) ;
#2835 = ORIENTED_EDGE ( 'NONE', *, *, #23758, .F. ) ;
#2836 = CARTESIAN_POINT ( 'NONE',  ( -1.511391232157798692, 24.58424253752448152, -1.760983478933511925 ) ) ;
#2837 = CARTESIAN_POINT ( 'NONE',  ( 5.578854890061005101, 14.64920222439000419, -2.552219347586000886 ) ) ;
#2838 = CARTESIAN_POINT ( 'NONE',  ( 12.00000000000000000, -6.865294675837238181, -5.791300988468927713 ) ) ;
#2839 = CARTESIAN_POINT ( 'NONE',  ( -20.14542920454665520, -4.627261388873439962, -8.028619099368466294 ) ) ;
#2840 = CARTESIAN_POINT ( 'NONE',  ( 12.73500142131000068, 5.721315692782000362, 7.730289442163000402 ) ) ;
#2841 = ORIENTED_EDGE ( 'NONE', *, *, #1985, .T. ) ;
#2842 = CARTESIAN_POINT ( 'NONE',  ( -11.84376649291999861, 8.442406968109999355, -11.81034824682000028 ) ) ;
#2843 = CARTESIAN_POINT ( 'NONE',  ( -1.672509921847626257, 24.50639765414753057, -3.652834497694422033 ) ) ;
#2844 = CARTESIAN_POINT ( 'NONE',  ( -12.50000000000000000, -10.59999999999999964, 0.000000000000000000 ) ) ;
#2845 = ADVANCED_FACE ( 'NONE', ( #8258, #15868 ), #19144, .F. ) ;
#2846 = EDGE_LOOP ( 'NONE', ( #5654, #20814, #22515, #3675, #21747, #1882, #23557, #7256, #1650, #1496 ) ) ;
#2847 = CARTESIAN_POINT ( 'NONE',  ( 4.000000000000000000, 26.50000000000000711, -0.3708744353061897980 ) ) ;
#2848 = CARTESIAN_POINT ( 'NONE',  ( 12.28022044530303347, 13.65679895895511109, 1.345730334339762857 ) ) ;
#2849 = DIRECTION ( 'NONE',  ( 0.000000000000000000, 0.000000000000000000, 1.000000000000000000 ) ) ;
#2850 = DIRECTION ( 'NONE',  ( -1.000000000000000000, 0.000000000000000000, 0.000000000000000000 ) ) ;
#2851 = CARTESIAN_POINT ( 'NONE',  ( 16.68568461312300499, 10.32051225367915492, -1.596948730429063046 ) ) ;
#2852 = CARTESIAN_POINT ( 'NONE',  ( 12.00000000000000355, -5.410480646876911770, -8.043393307973820683 ) ) ;
#2853 = DIRECTION ( 'NONE',  ( 1.000000000000000000, 0.000000000000000000, 0.000000000000000000 ) ) ;
#2854 = CARTESIAN_POINT ( 'NONE',  ( 22.25349774961999927, 7.219487340945000220, 8.632260055193999193 ) ) ;
#2855 = DIRECTION ( 'NONE',  ( 0.000000000000000000, 0.000000000000000000, -1.000000000000000000 ) ) ;
#2856 = CARTESIAN_POINT ( 'NONE',  ( -3.845736221939690225, 14.02535984897294696, -4.848784559987059595 ) ) ;
#2857 = ADVANCED_FACE ( 'NONE', ( #23258 ), #20344, .F. ) ;
#2858 = CARTESIAN_POINT ( 'NONE',  ( -1.115914872543483538, 30.33458863209825296, 1.849708372149318381 ) ) ;
#2859 = ORIENTED_EDGE ( 'NONE', *, *, #11485, .F. ) ;
#2860 = CARTESIAN_POINT ( 'NONE',  ( 21.00002833972000005, -2.896904163262000065, -9.930905325560999586 ) ) ;
#2861 = CARTESIAN_POINT ( 'NONE',  ( 3.999878274658704047, 28.13336607547242352, -1.519686587934146349 ) ) ;
#2862 = DIRECTION ( 'NONE',  ( 0.000000000000000000, -1.000000000000000000, 0.000000000000000000 ) ) ;
#2863 = CARTESIAN_POINT ( 'NONE',  ( -19.84098316496925918, 4.513343901832210570, 9.564988471992716512 ) ) ;
#2864 = CARTESIAN_POINT ( 'NONE',  ( 4.888224998722219716, 14.41767836092300215, 3.807294520224770551 ) ) ;
#2865 = CARTESIAN_POINT ( 'NONE',  ( -2.000000000000000000, 24.50000000000000000, -3.464101615137999968 ) ) ;
#2866 = ORIENTED_EDGE ( 'NONE', *, *, #10142, .T. ) ;
#2867 = EDGE_CURVE ( 'NONE', #1813, #22702, #21828, .T. ) ;
#2868 = CARTESIAN_POINT ( 'NONE',  ( -14.64203606142728908, 9.931845001584829191, 2.940492112398142233 ) ) ;
#2869 = CIRCLE ( 'NONE', #914, 1.399999999999999911 ) ;
#2870 = DIRECTION ( 'NONE',  ( -0.7071067811865969777, 0.7071067811864980568, 2.474839539219989905E-09 ) ) ;
#2871 = CARTESIAN_POINT ( 'NONE',  ( -0.04320196544907554947, 27.02713582543505666, 2.171338851202412989 ) ) ;
#2872 = DIRECTION ( 'NONE',  ( 1.000000000000000000, 0.000000000000000000, 0.000000000000000000 ) ) ;
#2873 = CARTESIAN_POINT ( 'NONE',  ( 0.000000000000000000, 17.00000000000000000, 0.000000000000000000 ) ) ;
#2874 = EDGE_CURVE ( 'NONE', #18875, #13184, #2896, .T. ) ;
#2875 = VERTEX_POINT ( 'NONE', #21586 ) ;
#2876 = DIRECTION ( 'NONE',  ( -1.000000000000000000, 0.000000000000000000, 0.000000000000000000 ) ) ;
#2877 = CARTESIAN_POINT ( 'NONE',  ( 12.02006424930999984, -10.30839584998999925, 1.075033486111000025 ) ) ;
#2878 = AXIS2_PLACEMENT_3D ( 'NONE', #8181, #8426, #8059 ) ;
#2879 = CARTESIAN_POINT ( 'NONE',  ( -23.20401199359000088, -10.10894130240999900, -3.455853891913000187 ) ) ;
#2880 = CARTESIAN_POINT ( 'NONE',  ( -15.62919348333999991, -1.476505563563000001, -10.70629720786000050 ) ) ;
#2881 = DIRECTION ( 'NONE',  ( 0.000000000000000000, -1.000000000000000000, 0.000000000000000000 ) ) ;
#2882 = CARTESIAN_POINT ( 'NONE',  ( 18.71437451746000136, -4.405870748760999156, -8.778983313941999711 ) ) ;
#2883 = CARTESIAN_POINT ( 'NONE',  ( -0.9392386595127586446, 28.45998959359454972, -1.999008173069681371 ) ) ;
#2884 = B_SPLINE_CURVE_WITH_KNOTS ( 'NONE', 3,
 ( #1185, #5073, #4825, #15938, #2887, #19601, #12211, #3009, #8578, #23333, #14141, #21536, #4949, #12334, #10637, #18024, #8213, #5298 ),
 .UNSPECIFIED., .F., .F.,
 ( 4, 2, 2, 2, 2, 2, 2, 2, 4 ),
 ( 0.000000000000000000, 0.1250000000000000278, 0.2500000000000000555, 0.3750000000000001110, 0.5000000000000001110, 0.6250000000000001110, 0.7500000000000002220, 0.8750000000000001110, 1.000000000000000000 ),
 .UNSPECIFIED. ) ;
#2885 = CARTESIAN_POINT ( 'NONE',  ( 20.40736763244999707, -7.483925214229000034, -6.133533836256000349 ) ) ;
#2886 = EDGE_CURVE ( 'NONE', #11065, #22774, #5000, .T. ) ;
#2887 = CARTESIAN_POINT ( 'NONE',  ( 15.42704166666666055, 7.250625443680725368, -5.572289352991960598 ) ) ;
#2888 = ORIENTED_EDGE ( 'NONE', *, *, #15839, .T. ) ;
#2889 = AXIS2_PLACEMENT_3D ( 'NONE', #6465, #14221, #15898 ) ;
#2890 = CARTESIAN_POINT ( 'NONE',  ( -2.131540934788977548, 13.91340213905352918, 5.742140983464480541 ) ) ;
#2891 = CARTESIAN_POINT ( 'NONE',  ( -1.978081431919000099, 28.60869850838000161, 1.107772814030999919 ) ) ;
#2892 = CARTESIAN_POINT ( 'NONE',  ( 4.000000000000000000, 26.20000000000000284, 2.309401076759000304 ) ) ;
#2893 = CARTESIAN_POINT ( 'NONE',  ( -1.590840130251000017, 27.70437716036000353, -1.862634475845999837 ) ) ;
#2894 = AXIS2_PLACEMENT_3D ( 'NONE', #10555, #1346, #17939 ) ;
#2895 = ORIENTED_EDGE ( 'NONE', *, *, #7191, .F. ) ;
#2896 = B_SPLINE_CURVE_WITH_KNOTS ( 'NONE', 3,
 ( #1702, #19883, #12730, #1229, #10563, #21930, #23376, #16106, #23510, #6794, #14536, #5230, #23853, #4873, #7145, #3298, #3058, #8870 ),
 .UNSPECIFIED., .F., .F.,
 ( 4, 2, 2, 2, 2, 2, 2, 2, 4 ),
 ( 0.000000000000000000, 0.1250000000000000555, 0.2500000000000001110, 0.3750000000000000555, 0.5000000000000000000, 0.6249999999999998890, 0.7499999999999998890, 0.8749999999999998890, 1.000000000000000000 ),
 .UNSPECIFIED. ) ;
#2897 = DIRECTION ( 'NONE',  ( 0.000000000000000000, -0.9999999999994555466, 1.043416718096953418E-06 ) ) ;
#2898 = CARTESIAN_POINT ( 'NONE',  ( 3.297306448684705682, 11.93904864444474789, -3.531362723138341320 ) ) ;
#2899 = PLANE ( 'NONE',  #5691 ) ;
#2900 = AXIS2_PLACEMENT_3D ( 'NONE', #8275, #6448, #4518 ) ;
#2901 = CARTESIAN_POINT ( 'NONE',  ( -1.802851389305008434, 26.49891402983596222, 1.731858503842447217 ) ) ;
#2902 = DIRECTION ( 'NONE',  ( -0.6979779633370118974, 0.000000000000000000, -0.7161192377641567575 ) ) ;
#2903 = EDGE_CURVE ( 'NONE', #4084, #5502, #17574, .T. ) ;
#2904 = EDGE_CURVE ( 'NONE', #21421, #16694, #861, .T. ) ;
#2905 = CARTESIAN_POINT ( 'NONE',  ( -12.33075721169000083, 13.48257539618999878, -7.785259987329999909 ) ) ;
#2906 = CARTESIAN_POINT ( 'NONE',  ( 0.6634078306992999829, 24.00000000000000000, -2.410371351092000403 ) ) ;
#2907 = CARTESIAN_POINT ( 'NONE',  ( 15.69656392131000011, 1.888996749216000026, -9.509257592937000680 ) ) ;
#2908 = CARTESIAN_POINT ( 'NONE',  ( 18.93485879530803118, 2.282263698320222911, 10.18192374699490799 ) ) ;
#2909 = VERTEX_POINT ( 'NONE', #12615 ) ;
#2910 = CARTESIAN_POINT ( 'NONE',  ( -10.90000000000000036, 1.358133300253999998E-14, 0.000000000000000000 ) ) ;
#2911 = CARTESIAN_POINT ( 'NONE',  ( 0.2527145128676999697, 30.46290016897999919, 2.328107194952999670 ) ) ;
#2912 = DIRECTION ( 'NONE',  ( 0.000000000000000000, -1.000000000000000000, 0.000000000000000000 ) ) ;
#2913 = CARTESIAN_POINT ( 'NONE',  ( -2.531476009669907601, 14.00394004275433524, -5.577390614649326395 ) ) ;
#2914 = ORIENTED_EDGE ( 'NONE', *, *, #10159, .F. ) ;
#2915 = DIRECTION ( 'NONE',  ( 1.000000000000000000, 0.000000000000000000, 0.000000000000000000 ) ) ;
#2916 = DIRECTION ( 'NONE',  ( -1.000000000000000000, 0.000000000000000000, 0.000000000000000000 ) ) ;
#2917 = CARTESIAN_POINT ( 'NONE',  ( 2.545098575468000224, 30.12522639263000102, 1.030125257387999982 ) ) ;
#2918 = ADVANCED_FACE ( 'NONE', ( #14315 ), #9062, .T. ) ;
#2919 = FACE_BOUND ( 'NONE', #7529, .T. ) ;
#2920 = EDGE_CURVE ( 'NONE', #8124, #12420, #16240, .T. ) ;
#2921 = CARTESIAN_POINT ( 'NONE',  ( 14.61516467955725851, 9.713890784730681460, -3.635657044371410684 ) ) ;
#2922 = CARTESIAN_POINT ( 'NONE',  ( -4.414959355983806510, 13.54502321037925228, 5.029880799536921465 ) ) ;
#2923 = DIRECTION ( 'NONE',  ( 1.000000000000000000, 0.000000000000000000, 0.000000000000000000 ) ) ;
#2924 = CARTESIAN_POINT ( 'NONE',  ( 4.649999999999999467, 15.00000000000000000, 0.000000000000000000 ) ) ;
#2925 = ORIENTED_EDGE ( 'NONE', *, *, #3934, .F. ) ;
#2926 = CARTESIAN_POINT ( 'NONE',  ( 4.143262790852083377, 12.32174769774581868, -2.404817559472536725 ) ) ;
#2927 = ORIENTED_EDGE ( 'NONE', *, *, #11455, .T. ) ;
#2928 = CARTESIAN_POINT ( 'NONE',  ( -0.7063789491035000756, 25.71876066959000084, 2.445197883720000132 ) ) ;
#2929 = DIRECTION ( 'NONE',  ( -1.000000000000000000, 0.000000000000000000, 0.000000000000000000 ) ) ;
#2930 = CARTESIAN_POINT ( 'NONE',  ( -0.5794485495992535151, 12.81494912436375877, 6.641564743694956974 ) ) ;
#2931 = AXIS2_PLACEMENT_3D ( 'NONE', #12827, #20330, #14634 ) ;
#2932 = CARTESIAN_POINT ( 'NONE',  ( 0.000000000000000000, 13.00000000000000000, 0.000000000000000000 ) ) ;
#2933 = DIRECTION ( 'NONE',  ( 0.000000000000000000, 0.000000000000000000, -1.000000000000000000 ) ) ;
#2934 = EDGE_LOOP ( 'NONE', ( #4494, #13395, #1567, #14429 ) ) ;
#2935 = CARTESIAN_POINT ( 'NONE',  ( 1.259047450927257339, 30.10086340285667106, 2.184465970885639763 ) ) ;
#2936 = CARTESIAN_POINT ( 'NONE',  ( -0.1017505424761079302, 26.49824549261836992, -2.396632052897438303 ) ) ;
#2937 = LINE ( 'NONE', #8265, #21043 ) ;
#2938 = ORIENTED_EDGE ( 'NONE', *, *, #4806, .T. ) ;
#2939 = CARTESIAN_POINT ( 'NONE',  ( -19.84656726529999915, 9.357477915406001046, -3.920807637256999989 ) ) ;
#2940 = DIRECTION ( 'NONE',  ( -1.000000000000000000, 0.000000000000000000, 0.000000000000000000 ) ) ;
#2941 = CARTESIAN_POINT ( 'NONE',  ( 23.99062354302999722, 6.216878364870000340, -12.50000000000000000 ) ) ;
#2942 = CARTESIAN_POINT ( 'NONE',  ( 14.90675817089161903, 10.32645797258115472, -0.4027543523436388218 ) ) ;
#2943 = CARTESIAN_POINT ( 'NONE',  ( 30.87226923053214378, 27.01856778792605240, -2.673746900119611247 ) ) ;
#2944 = AXIS2_PLACEMENT_3D ( 'NONE', #3071, #17720, #8519 ) ;
#2945 = CARTESIAN_POINT ( 'NONE',  ( 0.000000000000000000, 24.80000000000000426, 4.618802153517000519 ) ) ;
#2946 = DIRECTION ( 'NONE',  ( 0.000000000000000000, 1.000000000000000000, 0.000000000000000000 ) ) ;
#2947 = CARTESIAN_POINT ( 'NONE',  ( -3.583888380590997347, 12.05920279233998649, -3.176321221271000361 ) ) ;
#2948 = ORIENTED_EDGE ( 'NONE', *, *, #2410, .T. ) ;
#2949 = AXIS2_PLACEMENT_3D ( 'NONE', #10733, #23563, #8799 ) ;
#2950 = CARTESIAN_POINT ( 'NONE',  ( -6.249999999916000526, 15.09564573669999987, 3.212813967733000098 ) ) ;
#2951 = CARTESIAN_POINT ( 'NONE',  ( -1.668398882160119889, 29.31622934884095244, -1.371800779754721145 ) ) ;
#2952 = ORIENTED_EDGE ( 'NONE', *, *, #19783, .T. ) ;
#2953 = DIRECTION ( 'NONE',  ( 0.000000000000000000, 1.000000000000000000, 0.000000000000000000 ) ) ;
#2954 = CARTESIAN_POINT ( 'NONE',  ( -17.44374957678954985, -8.022022119424356390, -6.684027340921669946 ) ) ;
#2955 = ORIENTED_EDGE ( 'NONE', *, *, #22482, .T. ) ;
#2956 = CARTESIAN_POINT ( 'NONE',  ( 2.461510100158181391, 30.03430034141290150, -0.6707223322621249650 ) ) ;
#2957 = CARTESIAN_POINT ( 'NONE',  ( 5.640389443970001970, 14.19524044333999058, -2.282071340294998585 ) ) ;
#2958 = CARTESIAN_POINT ( 'NONE',  ( 6.696152422707000618, 26.50000000000000000, 6.000000000000000000 ) ) ;
#2959 = CARTESIAN_POINT ( 'NONE',  ( 24.28455689590321498, 3.990707743056026935, -12.50000000000000000 ) ) ;
#2960 = CARTESIAN_POINT ( 'NONE',  ( 13.41956408531000022, -7.835164430201999153, 6.443409769539999665 ) ) ;
#2961 = ORIENTED_EDGE ( 'NONE', *, *, #2419, .T. ) ;
#2962 = CARTESIAN_POINT ( 'NONE',  ( 2.504532394112000003E-14, 28.43419673618999965, 2.500000000000000000 ) ) ;
#2963 = CIRCLE ( 'NONE', #7200, 1.000000000000000666 ) ;
#2964 = FACE_OUTER_BOUND ( 'NONE', #7028, .T. ) ;
#2965 = CARTESIAN_POINT ( 'NONE',  ( -18.13088126894000141, 1.446686056264999920E-14, 0.000000000000000000 ) ) ;
#2966 = ORIENTED_EDGE ( 'NONE', *, *, #14275, .T. ) ;
#2967 = CARTESIAN_POINT ( 'NONE',  ( 11.59051697470852460, 8.994977951493066115, 9.420063436870602658 ) ) ;
#2968 = PLANE ( 'NONE',  #7688 ) ;
#2969 = CARTESIAN_POINT ( 'NONE',  ( -5.340660509843405457, 14.27930097228464135, -5.055472689471347536 ) ) ;
#2970 = CARTESIAN_POINT ( 'NONE',  ( 16.59721451432771033, 9.337922582797750337, -4.634226228450162743 ) ) ;
#2971 = CARTESIAN_POINT ( 'NONE',  ( -24.50000000000000000, 1.721664336791999924E-14, 0.000000000000000000 ) ) ;
#2972 = CARTESIAN_POINT ( 'NONE',  ( -14.48633711635905819, -11.53909476760599873, 5.013715100885081988 ) ) ;
#2973 = CIRCLE ( 'NONE', #18070, 0.09999999999999942268 ) ;
#2974 = CARTESIAN_POINT ( 'NONE',  ( -3.889659136885874613, 13.97224236195846636, -4.846263912825002684 ) ) ;
#2975 = CARTESIAN_POINT ( 'NONE',  ( 12.52688711657000020, 7.716878364870000340, -11.63397459621999985 ) ) ;
#2976 = CARTESIAN_POINT ( 'NONE',  ( -1.681629395837270557, 30.11728915368498605, -1.356799994207296800 ) ) ;
#2977 = ORIENTED_EDGE ( 'NONE', *, *, #5483, .T. ) ;
#2978 = CARTESIAN_POINT ( 'NONE',  ( 2.096382098643999825, 25.85732963143999896, -0.7353180384705999550 ) ) ;
#2979 = CARTESIAN_POINT ( 'NONE',  ( 21.38653020683999983, 9.007749467335999682, -5.108484126438000317 ) ) ;
#2980 = CARTESIAN_POINT ( 'NONE',  ( 23.44869471829550278, -3.059739909190946960, -10.14852769068212268 ) ) ;
#2981 = CONICAL_SURFACE ( 'NONE', #21158, 9.157130689899000586, 0.02565634000431304615 ) ;
#2982 = CARTESIAN_POINT ( 'NONE',  ( -1.199159982883566622, 23.61694849536621987, -1.744592755163365094 ) ) ;
#2983 = VERTEX_POINT ( 'NONE', #21816 ) ;
#2984 = ADVANCED_FACE ( 'NONE', ( #20000 ), #18074, .T. ) ;
#2985 = CARTESIAN_POINT ( 'NONE',  ( 2.207668724461689713, 24.00469357743359566, 0.4510245842454297938 ) ) ;
#2986 = CARTESIAN_POINT ( 'NONE',  ( 4.829988586904999437, 14.79876397742000016, 3.766541904039999888 ) ) ;
#2987 = B_SPLINE_CURVE_WITH_KNOTS ( 'NONE', 3,
 ( #20817, #9321, #22387, #13295 ),
 .UNSPECIFIED., .F., .F.,
 ( 4, 4 ),
 ( 0.000000000000000000, 1.000000000000000000 ),
 .UNSPECIFIED. ) ;
#2988 = CARTESIAN_POINT ( 'NONE',  ( -3.701981919174000435, 12.09302152519998330, -3.290687922835001000 ) ) ;
#2989 = VERTEX_POINT ( 'NONE', #12842 ) ;
#2990 = CARTESIAN_POINT ( 'NONE',  ( -16.03759792288471075, -1.727053351349761900, 10.25380015627600905 ) ) ;
#2991 = CARTESIAN_POINT ( 'NONE',  ( 0.000000000000000000, 7.000000000000000000, 0.000000000000000000 ) ) ;
#2992 = CIRCLE ( 'NONE', #16511, 4.750000000000000000 ) ;
#2993 = VERTEX_POINT ( 'NONE', #7382 ) ;
#2994 = LINE ( 'NONE', #17643, #6347 ) ;
#2995 = DIRECTION ( 'NONE',  ( 0.000000000000000000, 0.000000000000000000, 1.000000000000000000 ) ) ;
#2996 = AXIS2_PLACEMENT_3D ( 'NONE', #7622, #14764, #20350 ) ;
#2997 = DIRECTION ( 'NONE',  ( -1.000000000000000000, 0.000000000000000000, 0.000000000000000000 ) ) ;
#2998 = EDGE_CURVE ( 'NONE', #22108, #4259, #12657, .T. ) ;
#2999 = ORIENTED_EDGE ( 'NONE', *, *, #5856, .T. ) ;
#3000 = LINE ( 'NONE', #8570, #20563 ) ;
#3001 = AXIS2_PLACEMENT_3D ( 'NONE', #15537, #14095, #19433 ) ;
#3002 = CARTESIAN_POINT ( 'NONE',  ( -4.517065591395176938, 15.49914285584037899, -4.136658920617758639 ) ) ;
#3003 = CARTESIAN_POINT ( 'NONE',  ( -23.04342530862000160, -6.757663101931999705, -8.268912786219999589 ) ) ;
#3004 = CARTESIAN_POINT ( 'NONE',  ( -17.86362731101000278, -10.86714433699999915, 0.2447078565204000022 ) ) ;
#3005 = DIRECTION ( 'NONE',  ( 0.000000000000000000, -1.000000000000000000, 0.000000000000000000 ) ) ;
#3006 = CARTESIAN_POINT ( 'NONE',  ( 14.58369494525999954, -9.776545566456000813, -3.069771413624999834 ) ) ;
#3007 = CARTESIAN_POINT ( 'NONE',  ( -1.655756533096874872, 28.51299189722077898, -1.457120583913508183 ) ) ;
#3008 = CARTESIAN_POINT ( 'NONE',  ( 2.160826008357635164, 26.50000000000000355, -3.371248675920325955 ) ) ;
#3009 = CARTESIAN_POINT ( 'NONE',  ( 15.23808333333332676, 2.371926055385309429, -8.826501586951490452 ) ) ;
#3010 = VERTEX_POINT ( 'NONE', #7746 ) ;
#3011 = CARTESIAN_POINT ( 'NONE',  ( 2.798004395824331247, 14.07234475661186046, 5.448569188702180988 ) ) ;
#3012 = CARTESIAN_POINT ( 'NONE',  ( 1.664720809480999986, 27.43869850838000346, -1.538852087555999892 ) ) ;
#3013 = CIRCLE ( 'NONE', #12299, 14.43375672973999890 ) ;
#3014 = CARTESIAN_POINT ( 'NONE',  ( 0.000000000000000000, 30.00000000000000000, -2.399999999999951950 ) ) ;
#3015 = ADVANCED_FACE ( 'NONE', ( #20471, #22272 ), #1822, .F. ) ;
#3016 = CARTESIAN_POINT ( 'NONE',  ( -20.26481641072999906, 10.68114957034000057, 2.862104170669000247 ) ) ;
#3017 = B_SPLINE_CURVE_WITH_KNOTS ( 'NONE', 3,
 ( #23129, #19521, #15620, #11651, #23009, #9705, #17328, #21210, #4495, #15256, #4625, #4377, #6426, #8138, #19022, #17581, #21333, #19140, #15503, #22890, #17088, #486, #13811, #7888, #22648, #974, #8376, #2552, #6058, #9823, #20851, #15742, #2433, #6554 ),
 .UNSPECIFIED., .F., .F.,
 ( 4, 2, 2, 2, 2, 2, 2, 2, 2, 2, 2, 2, 2, 2, 2, 2, 4 ),
 ( 0.4963961610726058127, 0.5278714010055679529, 0.5593466409385301485, 0.5908218808714922332, 0.6222971208044543179, 0.6537723607374165136, 0.6852476006703787093, 0.7167228406033407939, 0.7481980805363028786, 0.7796733204692650743, 0.8111485604022272700, 0.8426238003351893546, 0.8740990402681514393, 0.9055742802011136350, 0.9370495201340758307, 0.9685247600670379153, 1.000000000000000000 ),
 .UNSPECIFIED. ) ;
#3018 = CARTESIAN_POINT ( 'NONE',  ( -4.273318845158264878, 12.24029060234036237, 2.275484052468874197 ) ) ;
#3019 = EDGE_LOOP ( 'NONE', ( #12858, #20645, #20176, #19727 ) ) ;
#3020 = CARTESIAN_POINT ( 'NONE',  ( -12.75000000000000000, 0.000000000000000000, 0.000000000000000000 ) ) ;
#3021 = CARTESIAN_POINT ( 'NONE',  ( 4.519733411219042374, 12.32701741422152431, -1.748064119505302161 ) ) ;
#3022 = CARTESIAN_POINT ( 'NONE',  ( -2.460016173531001549, 13.49435256317998366, 5.562971390105002634 ) ) ;
#3023 = CARTESIAN_POINT ( 'NONE',  ( -20.48555420454666987, -9.196981408831147675, 1.203755103560655515 ) ) ;
#3024 = FACE_OUTER_BOUND ( 'NONE', #17593, .T. ) ;
#3025 = EDGE_CURVE ( 'NONE', #12095, #21674, #7227, .T. ) ;
#3026 = DIRECTION ( 'NONE',  ( -1.000000000000000000, 0.000000000000000000, 0.000000000000000000 ) ) ;
#3027 = CARTESIAN_POINT ( 'NONE',  ( 2.000000000000000000, 31.00000000000000000, 0.000000000000000000 ) ) ;
#3028 = CIRCLE ( 'NONE', #15375, 2.500000000000000000 ) ;
#3029 = CARTESIAN_POINT ( 'NONE',  ( 12.73500142131000068, 5.721315692782000362, 7.730289442163000402 ) ) ;
#3030 = DIRECTION ( 'NONE',  ( 0.000000000000000000, -1.000000000000000000, 0.000000000000000000 ) ) ;
#3031 = ORIENTED_EDGE ( 'NONE', *, *, #11401, .F. ) ;
#3032 = CARTESIAN_POINT ( 'NONE',  ( -2.270871215252209030, 18.00000000000000000, 0.000000000000000000 ) ) ;
#3033 = CARTESIAN_POINT ( 'NONE',  ( -2.332700628984000435, 30.30361591766000018, -0.9867309859219000057 ) ) ;
#3034 = CARTESIAN_POINT ( 'NONE',  ( -2.474225017569000151, 23.42832970622999866, 1.120252420451000042 ) ) ;
#3035 = DIRECTION ( 'NONE',  ( -1.000000000000000000, 0.000000000000000000, 0.000000000000000000 ) ) ;
#3036 = B_SPLINE_CURVE_WITH_KNOTS ( 'NONE', 3,
 ( #23366, #1344, #1588, #18292, #5677, #8970, #23843, #7253, #11017 ),
 .UNSPECIFIED., .F., .F.,
 ( 4, 1, 2, 2, 4 ),
 ( 0.000000000000000000, 0.2499999999999994449, 0.3749999999999993894, 0.4999999999999993339, 1.000000000000000000 ),
 .UNSPECIFIED. ) ;
#3037 = ORIENTED_EDGE ( 'NONE', *, *, #13978, .T. ) ;
#3038 = EDGE_CURVE ( 'NONE', #3318, #17201, #12428, .T. ) ;
#3040 = VECTOR ( 'NONE', #22225, 1000.000000000000114 ) ;
#3039 = DIRECTION ( 'NONE',  ( 9.309561455062000780E-11, 0.000000000000000000, -1.000000000000000000 ) ) ;
#3041 = CARTESIAN_POINT ( 'NONE',  ( -24.50000000000000000, 2.324045842668999493E-14, 12.50000000000000000 ) ) ;
#3042 = FACE_OUTER_BOUND ( 'NONE', #13242, .T. ) ;
#3043 = CARTESIAN_POINT ( 'NONE',  ( -11.72636993442999831, 14.27363006556999991, 0.000000000000000000 ) ) ;
#3044 = CARTESIAN_POINT ( 'NONE',  ( 16.81746331405949135, 5.745323216197852467, 8.703258724007747915 ) ) ;
#3045 = CARTESIAN_POINT ( 'NONE',  ( -4.177414563858471652, 13.69652605315409488, 4.902318025240887778 ) ) ;
#3046 = DIRECTION ( 'NONE',  ( -1.000000000000000000, 0.000000000000000000, 0.000000000000000000 ) ) ;
#3047 = EDGE_CURVE ( 'NONE', #1220, #19976, #1043, .T. ) ;
#3048 = DIRECTION ( 'NONE',  ( 0.000000000000000000, -1.000000000000000000, 0.000000000000000000 ) ) ;
#3049 = ORIENTED_EDGE ( 'NONE', *, *, #3923, .F. ) ;
#3050 = DIRECTION ( 'NONE',  ( 1.000000000000000000, 0.000000000000000000, 0.000000000000000000 ) ) ;
#3051 = EDGE_CURVE ( 'NONE', #23046, #4988, #17687, .T. ) ;
#3052 = CARTESIAN_POINT ( 'NONE',  ( 2.920483249375370960, 11.94533022032288727, -3.796384527241723816 ) ) ;
#3053 = ORIENTED_EDGE ( 'NONE', *, *, #7068, .T. ) ;
#3054 = CARTESIAN_POINT ( 'NONE',  ( -0.04357916811771000293, 24.95238759480999846, 2.544809683028999903 ) ) ;
#3055 = CYLINDRICAL_SURFACE ( 'NONE', #6999, 2.500000000000000000 ) ;
#3056 = CARTESIAN_POINT ( 'NONE',  ( -0.4175917513579801565, 12.80961402668161142, 6.651874616197407164 ) ) ;
#3057 = CARTESIAN_POINT ( 'NONE',  ( 6.215921278351865809, 13.80668456282085366, -1.138992957140015250 ) ) ;
#3058 = CARTESIAN_POINT ( 'NONE',  ( -2.500000000000000444, 27.98333333333333428, -0.3272492347489320275 ) ) ;
#3059 = CIRCLE ( 'NONE', #19688, 4.750000000000000000 ) ;
#3060 = CARTESIAN_POINT ( 'NONE',  ( -6.043487373412999908, 16.34784519966000005, -1.000000006055999924 ) ) ;
#3061 = EDGE_CURVE ( 'NONE', #14234, #16706, #3385, .T. ) ;
#3062 = ORIENTED_EDGE ( 'NONE', *, *, #12245, .T. ) ;
#3063 = ADVANCED_FACE ( 'NONE', ( #7498 ), #9208, .T. ) ;
#3064 = TOROIDAL_SURFACE ( 'NONE', #20832, 5.625000000000000000, 0.5000000000000000000 ) ;
#3065 = CARTESIAN_POINT ( 'NONE',  ( -14.00000000000000533, -10.15903121243555773, -1.673958311142742073 ) ) ;
#3066 = CONICAL_SURFACE ( 'NONE', #20068, 13.23032192316000000, 1.235249617460683957 ) ;
#3067 = CARTESIAN_POINT ( 'NONE',  ( 0.4755391251864483082, 26.25858828695499270, 2.107219116345798948 ) ) ;
#3068 = CARTESIAN_POINT ( 'NONE',  ( -3.999895459877826465, 24.70780860099995380, 1.909390889640791622 ) ) ;
#3069 = VERTEX_POINT ( 'NONE', #16942 ) ;
#3070 = CARTESIAN_POINT ( 'NONE',  ( -23.93304557145999922, 10.81351501108999891, -3.289488343111999669 ) ) ;
#3071 = CARTESIAN_POINT ( 'NONE',  ( -10.35615758860000035, 0.000000000000000000, 0.000000000000000000 ) ) ;
#3072 = CARTESIAN_POINT ( 'NONE',  ( 14.97401178964219959, 10.12462245865840949, 2.061518227450690244 ) ) ;
#3073 = CONICAL_SURFACE ( 'NONE', #13481, 9.136555860486998526, 0.02565634000431304615 ) ;
#3074 = CARTESIAN_POINT ( 'NONE',  ( -0.3656491329547000291, 28.60167447434999843, 2.243838195847999817 ) ) ;
#3075 = CARTESIAN_POINT ( 'NONE',  ( 13.59694017449214165, 6.847023289163344018, -5.872291703794573436 ) ) ;
#3076 = CARTESIAN_POINT ( 'NONE',  ( -4.665938679690996516, 12.51338962337001703, -0.7728731416223998396 ) ) ;
#3077 = ORIENTED_EDGE ( 'NONE', *, *, #7041, .T. ) ;
#3078 = DIRECTION ( 'NONE',  ( 0.000000000000000000, -1.000000000000000000, 0.000000000000000000 ) ) ;
#3079 = CIRCLE ( 'NONE', #17767, 4.000000000000000000 ) ;
#3080 = CARTESIAN_POINT ( 'NONE',  ( -1.053212785059553180, 29.53888443595877789, 1.885826740177577676 ) ) ;
#3081 = ORIENTED_EDGE ( 'NONE', *, *, #14325, .T. ) ;
#3082 = LINE ( 'NONE', #12280, #14568 ) ;
#3083 = CARTESIAN_POINT ( 'NONE',  ( -16.37300014439912133, 3.220437795823801075, 10.06239832674213552 ) ) ;
#3084 = AXIS2_PLACEMENT_3D ( 'NONE', #2384, #6135, #14972 ) ;
#3085 = ORIENTED_EDGE ( 'NONE', *, *, #18004, .F. ) ;
#3086 = CARTESIAN_POINT ( 'NONE',  ( 6.265924793058000652, 13.58761645048999966, -2.214804771343001910 ) ) ;
#3087 = CARTESIAN_POINT ( 'NONE',  ( 11.99999999999999822, -1.594904923283001263, -8.836587722619364982 ) ) ;
#3088 = AXIS2_PLACEMENT_3D ( 'NONE', #4126, #597, #15497 ) ;
#3089 = CARTESIAN_POINT ( 'NONE',  ( 17.00514426052999895, 0.2856091294997000207, 11.08057831931000159 ) ) ;
#3090 = CARTESIAN_POINT ( 'NONE',  ( 13.30987658531000051, -4.885510779899000511, 8.887104416848000454 ) ) ;
#3091 = EDGE_CURVE ( 'NONE', #18033, #6675, #9446, .T. ) ;
#3092 = VERTEX_POINT ( 'NONE', #12952 ) ;
#3093 = CARTESIAN_POINT ( 'NONE',  ( -9.196381492921000600, -10.96796587088999964, -9.511275453079001352 ) ) ;
#3094 = CARTESIAN_POINT ( 'NONE',  ( 0.000000000000000000, -1.550000000000000044, 0.000000000000000000 ) ) ;
#3095 = CARTESIAN_POINT ( 'NONE',  ( 0.000000000000000000, 18.00000000000000000, 0.000000000000000000 ) ) ;
#3096 = ORIENTED_EDGE ( 'NONE', *, *, #2750, .T. ) ;
#3097 = CARTESIAN_POINT ( 'NONE',  ( -23.71548049068999831, -4.708188689841001029, -8.512973244356000890 ) ) ;
#3098 = CARTESIAN_POINT ( 'NONE',  ( 0.000000000000000000, 13.04999996922999905, 0.000000000000000000 ) ) ;
#3099 = CARTESIAN_POINT ( 'NONE',  ( 22.88230379277824511, -10.58571745970539624, -0.03397870593635089059 ) ) ;
#3100 = DIRECTION ( 'NONE',  ( 1.000000000000000000, 0.000000000000000000, 0.000000000000000000 ) ) ;
#3102 = CARTESIAN_POINT ( 'NONE',  ( 17.10182080017775519, 2.899594746005321966, 10.01006028584902197 ) ) ;
#3101 = VECTOR ( 'NONE', #14379, 1000.000000000000000 ) ;
#3103 = VECTOR ( 'NONE', #21801, 1000.000000000000000 ) ;
#3104 = CARTESIAN_POINT ( 'NONE',  ( -18.71524577250666965, -2.395516608000527015, 8.913312826780673603 ) ) ;
#3105 = CARTESIAN_POINT ( 'NONE',  ( 0.000000000000000000, 17.89999999999999858, 0.000000000000000000 ) ) ;
#3106 = B_SPLINE_CURVE_WITH_KNOTS ( 'NONE', 3,
 ( #16326, #9422, #19977, #16793, #12821, #3397, #16562, #12927 ),
 .UNSPECIFIED., .F., .F.,
 ( 4, 2, 2, 4 ),
 ( 0.000000000000000000, 0.2500000000000000000, 0.5000000000000000000, 1.000000000000000000 ),
 .UNSPECIFIED. ) ;
#3107 = CARTESIAN_POINT ( 'NONE',  ( -3.782540744202022243, 14.10894914716129556, -4.859551560401516035 ) ) ;
#3108 = APPLICATION_CONTEXT ( 'automotive_design' ) ;
#3109 = CARTESIAN_POINT ( 'NONE',  ( -2.158863305921206344, 30.19885671959407603, -0.08137547947002730930 ) ) ;
#3110 = ORIENTED_EDGE ( 'NONE', *, *, #20635, .T. ) ;
#3111 = CARTESIAN_POINT ( 'NONE',  ( -2.187279742372999713, 25.36874527294000359, -0.8192853498630000564 ) ) ;
#3112 = CARTESIAN_POINT ( 'NONE',  ( 24.90575349395000160, -9.343402930240999993, -5.725328257854999769 ) ) ;
#3113 = CARTESIAN_POINT ( 'NONE',  ( 22.73936012672840690, -4.034463466300610257, 9.782371928200333855 ) ) ;
#3114 = DIRECTION ( 'NONE',  ( 0.000000000000000000, -0.7071067811866525998, -0.7071067811864425456 ) ) ;
#3115 = ORIENTED_EDGE ( 'NONE', *, *, #168, .T. ) ;
#3116 = FACE_OUTER_BOUND ( 'NONE', #11330, .T. ) ;
#3117 = CARTESIAN_POINT ( 'NONE',  ( 4.894061048423400173, 14.39961068744026562, 3.811571210762304318 ) ) ;
#3118 = CARTESIAN_POINT ( 'NONE',  ( 4.925062053240003124, 12.50686037410001639, -0.5310971773938999441 ) ) ;
#3119 = ORIENTED_EDGE ( 'NONE', *, *, #3366, .F. ) ;
#3120 = CARTESIAN_POINT ( 'NONE',  ( -14.80950348480317658, 9.924210800638553209, -2.985472924579720910 ) ) ;
#3121 = DIRECTION ( 'NONE',  ( -2.945128176746998816E-08, 0.9999999999999996669, -2.371622976689998485E-09 ) ) ;
#3122 = ORIENTED_EDGE ( 'NONE', *, *, #23465, .F. ) ;
#3123 = CIRCLE ( 'NONE', #1944, 3.000000000000000000 ) ;
#3124 = CARTESIAN_POINT ( 'NONE',  ( -1.921811817508991993, 26.76825189519908577, -1.007139915559144283 ) ) ;
#3125 = CARTESIAN_POINT ( 'NONE',  ( 0.000000000000000000, 0.000000000000000000, 0.000000000000000000 ) ) ;
#3126 = DIRECTION ( 'NONE',  ( 0.000000000000000000, 1.000000000000000000, 0.000000000000000000 ) ) ;
#3127 = ORIENTED_EDGE ( 'NONE', *, *, #18558, .F. ) ;
#3128 = CARTESIAN_POINT ( 'NONE',  ( -19.00198616926667228, -2.679675940451125893, 8.823058184319245711 ) ) ;
#3129 = CARTESIAN_POINT ( 'NONE',  ( -3.940066807388778791, 14.83395602534511148, -4.689820734438498562 ) ) ;
#3130 = CARTESIAN_POINT ( 'NONE',  ( -24.70589367413000303, 9.599129830737000546, 1.290551844122999725 ) ) ;
#3131 = ADVANCED_FACE ( 'NONE', ( #225 ), #16586, .F. ) ;
#3132 = CARTESIAN_POINT ( 'NONE',  ( -18.47301835491999711, 5.805793625715000239, 9.209612613527001557 ) ) ;
#3133 = CARTESIAN_POINT ( 'NONE',  ( 22.11616666666665409, -8.072809104850792394, -4.652730915293407321 ) ) ;
#3134 = CARTESIAN_POINT ( 'NONE',  ( 14.78681994525999954, -5.472050788572000002, -8.670468866855999934 ) ) ;
#3135 = CARTESIAN_POINT ( 'NONE',  ( -1.211852003089728846, 27.92996655705957920, 1.828385414783800567 ) ) ;
#3136 = FACE_OUTER_BOUND ( 'NONE', #21640, .T. ) ;
#3137 = CARTESIAN_POINT ( 'NONE',  ( 5.607952975149999908, 13.81675705620000016, -3.376495290877999711 ) ) ;
#3138 = ORIENTED_EDGE ( 'NONE', *, *, #19897, .F. ) ;
#3139 = CARTESIAN_POINT ( 'NONE',  ( -17.68897087121334977, 9.125215568721371184, 1.194614872368663372 ) ) ;
#3140 = CARTESIAN_POINT ( 'NONE',  ( 0.08622555209230960138, 13.69124592427118969, 6.124469631175590401 ) ) ;
#3141 = CARTESIAN_POINT ( 'NONE',  ( 0.4658180156273000194, 28.77119850838000303, 2.070238309910999774 ) ) ;
#3142 = CARTESIAN_POINT ( 'NONE',  ( 2.321186682587942141, 26.50000000000000355, 3.278664397485417492 ) ) ;
#3143 = EDGE_CURVE ( 'NONE', #20723, #6198, #3615, .T. ) ;
#3144 = CARTESIAN_POINT ( 'NONE',  ( -0.7105796827303000329, 28.77687716036000154, 2.343805879471000164 ) ) ;
#3145 = VECTOR ( 'NONE', #15592, 1000.000000000000114 ) ;
#3146 = CARTESIAN_POINT ( 'NONE',  ( -8.099999999999999645, 1.323843189878000027E-14, 0.000000000000000000 ) ) ;
#3147 = VERTEX_POINT ( 'NONE', #5459 ) ;
#3148 = FACE_OUTER_BOUND ( 'NONE', #6184, .T. ) ;
#3149 = CARTESIAN_POINT ( 'NONE',  ( 4.420750779110104389, 12.29170844221592951, -1.979016023043961736 ) ) ;
#3150 = CARTESIAN_POINT ( 'NONE',  ( -10.86679200004126677, 15.33979541265035174, 1.708982890173643909 ) ) ;
#3151 = CARTESIAN_POINT ( 'NONE',  ( 1.612461263175861692, 6.966911249336811274, 0.6814213867173207761 ) ) ;
#3152 = CARTESIAN_POINT ( 'NONE',  ( -1.592810637863762091, 30.55640641325078377, -1.866744843515978802 ) ) ;
#3153 = CARTESIAN_POINT ( 'NONE',  ( -14.45834475453999879, 5.064797291421999859, 10.11313827054000036 ) ) ;
#3154 = CARTESIAN_POINT ( 'NONE',  ( 17.23218892130999791, -6.764005061571999988, -7.001918906472000437 ) ) ;
#3155 = CARTESIAN_POINT ( 'NONE',  ( 18.58051607384739867, 10.35305503824381645, 1.237856399541606311 ) ) ;
#3156 = EDGE_CURVE ( 'NONE', #13296, #15891, #23861, .T. ) ;
#3157 = VERTEX_POINT ( 'NONE', #15112 ) ;
#3158 = CARTESIAN_POINT ( 'NONE',  ( -22.68286091209157362, 7.357512616696472385, 5.643998677357938476 ) ) ;
#3159 = CARTESIAN_POINT ( 'NONE',  ( 2.066640458449999773, 30.83305368145999736, -1.464273823065999958 ) ) ;
#3160 = CARTESIAN_POINT ( 'NONE',  ( 0.000000000000000000, 22.00131761696259503, 0.000000000000000000 ) ) ;
#3161 = CARTESIAN_POINT ( 'NONE',  ( -3.644450799678000230, 14.33206891749000000, -4.922778709793999674 ) ) ;
#3162 = ORIENTED_EDGE ( 'NONE', *, *, #14438, .F. ) ;
#3163 = DIRECTION ( 'NONE',  ( 0.000000000000000000, -0.7071067811866525998, -0.7071067811864425456 ) ) ;
#3164 = FACE_OUTER_BOUND ( 'NONE', #5617, .T. ) ;
#3165 = FACE_OUTER_BOUND ( 'NONE', #16934, .T. ) ;
#3166 = CARTESIAN_POINT ( 'NONE',  ( 0.7867367962552690441, 24.50000000000000000, -2.267387309971103271 ) ) ;
#3167 = CARTESIAN_POINT ( 'NONE',  ( 15.22846303346806707, -2.020663429760869878, 10.33544534940901194 ) ) ;
#3168 = DIRECTION ( 'NONE',  ( 0.4226182617407188702, 0.000000000000000000, 0.9063077870366409439 ) ) ;
#3169 = CARTESIAN_POINT ( 'NONE',  ( -3.284923493671003669, 11.90416970545999931, 3.676126646792003960 ) ) ;
#3170 = ADVANCED_FACE ( 'NONE', ( #343 ), #18530, .F. ) ;
#3171 = CARTESIAN_POINT ( 'NONE',  ( 20.17074770046333043, -5.646920343229677286, 7.348150695498397056 ) ) ;
#3172 = ORIENTED_EDGE ( 'NONE', *, *, #12517, .F. ) ;
#3173 = PLANE ( 'NONE',  #2894 ) ;
#3174 = CARTESIAN_POINT ( 'NONE',  ( 0.6838519463944332522, 24.63336607547026702, -4.223839491861407502 ) ) ;
#3175 = ORIENTED_EDGE ( 'NONE', *, *, #6427, .T. ) ;
#3176 = CARTESIAN_POINT ( 'NONE',  ( -2.281413340844999915, 24.81304703576000037, 1.128321157715000078 ) ) ;
#3177 = CARTESIAN_POINT ( 'NONE',  ( 4.818326428766001257, 14.92945012152000928, 3.793178214860002839 ) ) ;
#3178 = DIRECTION ( 'NONE',  ( 1.000000000000000000, 0.000000000000000000, 0.000000000000000000 ) ) ;
#3179 = CARTESIAN_POINT ( 'NONE',  ( 6.183697154463740020, 13.95082363276063653, -0.7065469572563792822 ) ) ;
#3180 = CARTESIAN_POINT ( 'NONE',  ( -5.857053599681002254, 15.76999461102998445, -1.550034662246998929 ) ) ;
#3181 = ADVANCED_FACE ( 'NONE', ( #9327 ), #5917, .T. ) ;
#3182 = CARTESIAN_POINT ( 'NONE',  ( -6.046837210729000489, 16.30334039894000142, -1.000000000000000000 ) ) ;
#3183 = VERTEX_POINT ( 'NONE', #23100 ) ;
#3184 = CARTESIAN_POINT ( 'NONE',  ( -4.000000000000000000, 29.69999999999999929, -2.309401076759000304 ) ) ;
#3185 = CARTESIAN_POINT ( 'NONE',  ( 13.21250000000000036, 0.000000000000000000, 0.000000000000000000 ) ) ;
#3186 = DIRECTION ( 'NONE',  ( 0.5000000000000169864, 0.000000000000000000, 0.8660254037844289376 ) ) ;
#3187 = EDGE_CURVE ( 'NONE', #15169, #4052, #6454, .T. ) ;
#3188 = ORIENTED_EDGE ( 'NONE', *, *, #22713, .T. ) ;
#3189 = CARTESIAN_POINT ( 'NONE',  ( -21.80412305057999944, 10.70889992142000047, -0.5279559311888000206 ) ) ;
#3190 = CARTESIAN_POINT ( 'NONE',  ( -0.7783053373570000266, 28.00000000000000000, 5.000000000000000000 ) ) ;
#3191 = CARTESIAN_POINT ( 'NONE',  ( 15.16527071506006941, 6.736440203948466099, 7.842709918793921098 ) ) ;
#3192 = CARTESIAN_POINT ( 'NONE',  ( -12.24999999459000044, 1.554281285377000029E-14, 0.000000000000000000 ) ) ;
#3193 = CARTESIAN_POINT ( 'NONE',  ( -1.649410120653000078, 30.80057471234000133, -1.407032441706000059 ) ) ;
#3194 = CARTESIAN_POINT ( 'NONE',  ( -22.50811508569069730, -6.110212329431499612, 6.967324166022520693 ) ) ;
#3195 = CARTESIAN_POINT ( 'NONE',  ( -3.848016993207002301, 12.29094384469000012, -2.779960707798002417 ) ) ;
#3196 = VERTEX_POINT ( 'NONE', #22744 ) ;
#3197 = B_SPLINE_CURVE_WITH_KNOTS ( 'NONE', 3,
 ( #21602, #19163, #8398, #8526, #6327, #12277, #13710, #13835, #19666, #12154 ),
 .UNSPECIFIED., .F., .F.,
 ( 4, 2, 2, 2, 4 ),
 ( 0.2414086770563061979, 0.4310565077922296484, 0.6207043385281530989, 0.8103521692640764940, 1.000000000000000000 ),
 .UNSPECIFIED. ) ;
#3198 = CARTESIAN_POINT ( 'NONE',  ( 24.25008227645999881, -9.630770167580999797, 0.000000000000000000 ) ) ;
#3199 = EDGE_CURVE ( 'NONE', #21988, #10806, #20769, .T. ) ;
#3200 = ORIENTED_EDGE ( 'NONE', *, *, #23093, .T. ) ;
#3201 = CARTESIAN_POINT ( 'NONE',  ( -1.750000000000000000, 7.000000000000000000, 0.000000000000000000 ) ) ;
#3202 = FACE_OUTER_BOUND ( 'NONE', #21824, .T. ) ;
#3203 = VERTEX_POINT ( 'NONE', #4233 ) ;
#3204 = CARTESIAN_POINT ( 'NONE',  ( 61.60588651278290939, 35.51856778792605240, -1.000000000000000000 ) ) ;
#3205 = CARTESIAN_POINT ( 'NONE',  ( 11.12576011241361940, -11.44859199040162068, -5.170472096576233412 ) ) ;
#3206 = CARTESIAN_POINT ( 'NONE',  ( -4.814895406027281055, 13.26421056701085099, -5.692049281717411091 ) ) ;
#3207 = CARTESIAN_POINT ( 'NONE',  ( 17.76077715286999847, -0.4685653280873000037, -11.09506330460999912 ) ) ;
#3208 = CARTESIAN_POINT ( 'NONE',  ( 1.812579491195999815, 27.28006359724000163, -1.675531247043999805 ) ) ;
#3209 = CARTESIAN_POINT ( 'NONE',  ( 13.63893908531000143, -10.12407100975999974, -0.7263252697377000633 ) ) ;
#3210 = VERTEX_POINT ( 'NONE', #18995 ) ;
#3211 = B_SPLINE_CURVE_WITH_KNOTS ( 'NONE', 3,
 ( #9233, #11885, #22646, #849, #17580, #15254, #4375, #6304, #11529, #6056, #11765, #11649, #2550 ),
 .UNSPECIFIED., .F., .F.,
 ( 4, 2, 1, 1, 1, 2, 2, 4 ),
 ( 0.000000000000000000, 0.2500000000000019429, 0.3750000000000021649, 0.4375000000000027200, 0.4687500000000027756, 0.4843750000000025535, 0.5000000000000023315, 1.000000000000000000 ),
 .UNSPECIFIED. ) ;
#3212 = CARTESIAN_POINT ( 'NONE',  ( -9.909138992921000977, 9.357018744401999655, 11.09985848640999961 ) ) ;
#3213 = CARTESIAN_POINT ( 'NONE',  ( 13.49999999999999822, 8.294162734344720178, -4.272258766888964665 ) ) ;
#3214 = LINE ( 'NONE', #17744, #8830 ) ;
#3215 = EDGE_CURVE ( 'NONE', #22068, #6244, #17608, .T. ) ;
#3216 = VERTEX_POINT ( 'NONE', #10166 ) ;
#3217 = CYLINDRICAL_SURFACE ( 'NONE', #20834, 2.000000000000000000 ) ;
#3218 = EDGE_CURVE ( 'NONE', #4867, #22108, #19629, .T. ) ;
#3219 = CARTESIAN_POINT ( 'NONE',  ( 11.31235608934058412, 9.572705071893905071, 8.419524251273594828 ) ) ;
#3220 = CARTESIAN_POINT ( 'NONE',  ( 22.49991417170085484, -2.603443972844405874, 10.25004708077911708 ) ) ;
#3221 = AXIS2_PLACEMENT_3D ( 'NONE', #14069, #21463, #15988 ) ;
#3222 = CARTESIAN_POINT ( 'NONE',  ( -4.917862031230266773, 13.52432712154163141, -5.676368724613010563 ) ) ;
#3223 = CARTESIAN_POINT ( 'NONE',  ( 16.29049680864105198, 0.4916202364665146485, -10.35987764636037056 ) ) ;
#3224 = CARTESIAN_POINT ( 'NONE',  ( 12.00000000000000000, 0.000000000000000000, 1.045589212608000028E-14 ) ) ;
#3225 = CARTESIAN_POINT ( 'NONE',  ( 2.293942080512999748, 30.64047076207999964, -0.4768116971341999633 ) ) ;
#3226 = CARTESIAN_POINT ( 'NONE',  ( 18.62128936713000371, -9.149140698829999252, 0.000000000000000000 ) ) ;
#3227 = CARTESIAN_POINT ( 'NONE',  ( 1.338211323675440934, 29.91862812200778521, -1.695402813922068930 ) ) ;
#3228 = EDGE_CURVE ( 'NONE', #9936, #6330, #4469, .T. ) ;
#3229 = EDGE_LOOP ( 'NONE', ( #20, #19235, #2546, #18356 ) ) ;
#3230 = CARTESIAN_POINT ( 'NONE',  ( 11.45478115326000612, 12.39608915219456442, -3.529209591797321632 ) ) ;
#3231 = CARTESIAN_POINT ( 'NONE',  ( 4.000000000000000000, 28.00000000000000000, 0.000000000000000000 ) ) ;
#3232 = CARTESIAN_POINT ( 'NONE',  ( 0.000000000000000000, 29.69999999999999929, -4.618802153517000519 ) ) ;
#3233 = ORIENTED_EDGE ( 'NONE', *, *, #17032, .F. ) ;
#3234 = CARTESIAN_POINT ( 'NONE',  ( 6.696152422707000618, 29.50000000000000000, 115.0195023120000002 ) ) ;
#3235 = CARTESIAN_POINT ( 'NONE',  ( -4.954596429287999371, 13.56914355584999754, 5.779622067328999080 ) ) ;
#3236 = CARTESIAN_POINT ( 'NONE',  ( 4.911774765700998913, 12.43823212697000535, 0.1548528812091000406 ) ) ;
#3237 = ORIENTED_EDGE ( 'NONE', *, *, #23888, .F. ) ;
#3238 = CARTESIAN_POINT ( 'NONE',  ( 16.87668875730999929, -8.405545991651999671, -3.781450583054000170 ) ) ;
#3239 = ORIENTED_EDGE ( 'NONE', *, *, #17155, .T. ) ;
#3240 = CARTESIAN_POINT ( 'NONE',  ( 1.613996465941623493, 27.32300317427615965, -1.453135498617304178 ) ) ;
#3241 = CARTESIAN_POINT ( 'NONE',  ( 0.5500000000000000444, 1.217911241751999838E-14, 0.000000000000000000 ) ) ;
#3242 = ORIENTED_EDGE ( 'NONE', *, *, #20373, .F. ) ;
#3243 = LINE ( 'NONE', #10628, #443 ) ;
#3244 = CARTESIAN_POINT ( 'NONE',  ( 5.699442596042000098, 1.578914512950999657E-14, 0.000000000000000000 ) ) ;
#3245 = CARTESIAN_POINT ( 'NONE',  ( -23.31260609398000128, -6.433678087575999349, -7.872534309770998995 ) ) ;
#3246 = CARTESIAN_POINT ( 'NONE',  ( -16.71089566058999765, -1.947775803553999818, 10.11646046336000104 ) ) ;
#3247 = CARTESIAN_POINT ( 'NONE',  ( 19.24399999999999977, 9.165120680968000144, 0.000000000000000000 ) ) ;
#3248 = CARTESIAN_POINT ( 'NONE',  ( -23.05782846884435955, -10.51579617812587131, -1.069715151266978692 ) ) ;
#3249 = CARTESIAN_POINT ( 'NONE',  ( -0.7981348345002412525, 27.95646770889779376, 2.019361405941054954 ) ) ;
#3250 = CARTESIAN_POINT ( 'NONE',  ( -14.25243324638999809, 13.93375672974000068, 0.8660254037843999608 ) ) ;
#3251 = DIRECTION ( 'NONE',  ( 1.000000000000000000, 0.000000000000000000, 0.000000000000000000 ) ) ;
#3252 = ORIENTED_EDGE ( 'NONE', *, *, #12194, .F. ) ;
#3253 = FACE_OUTER_BOUND ( 'NONE', #6502, .T. ) ;
#3254 = CARTESIAN_POINT ( 'NONE',  ( 0.000000000000000000, -9.000000000000000000, 0.000000000000000000 ) ) ;
#3256 = VECTOR ( 'NONE', #5978, 1000.000000000000000 ) ;
#3255 = CARTESIAN_POINT ( 'NONE',  ( 2.169172474974999876, 25.78119850838000460, -0.6576354733792000307 ) ) ;
#3257 = CIRCLE ( 'NONE', #23743, 4.649999999999999467 ) ;
#3258 = CARTESIAN_POINT ( 'NONE',  ( 0.000000000000000000, 9.000000000000000000, 0.000000000000000000 ) ) ;
#3259 = CARTESIAN_POINT ( 'NONE',  ( -23.75312892322000025, 3.479588606389999672, 10.59591538551999790 ) ) ;
#3260 = CARTESIAN_POINT ( 'NONE',  ( -4.747617524593668925, 12.41110054352763292, 0.9834176323472247905 ) ) ;
#3261 = EDGE_LOOP ( 'NONE', ( #16125, #20060, #20371, #9649, #15436 ) ) ;
#3262 = PRODUCT_RELATED_PRODUCT_CATEGORY ( 'part', '', ( #17128 ) ) ;
#3263 = CARTESIAN_POINT ( 'NONE',  ( 0.000000000000000000, 24.29999999999999716, 0.000000000000000000 ) ) ;
#3264 = CARTESIAN_POINT ( 'NONE',  ( -24.37124162822026463, -2.557079873875873322, -12.50000271512792871 ) ) ;
#3265 = CARTESIAN_POINT ( 'NONE',  ( -10.29381500303638930, 15.72616211534351471, 1.189143564266787578 ) ) ;
#3266 = CARTESIAN_POINT ( 'NONE',  ( 11.82347178278407718, 0.1432880675219483646, -8.999235042547903518 ) ) ;
#3267 = CIRCLE ( 'NONE', #18715, 4.750000000000000000 ) ;
#3268 = ORIENTED_EDGE ( 'NONE', *, *, #17430, .T. ) ;
#3269 = DIRECTION ( 'NONE',  ( 1.000000000000000000, 0.000000000000000000, 0.000000000000000000 ) ) ;
#3270 = DIRECTION ( 'NONE',  ( 0.000000000000000000, 0.000000000000000000, 1.000000000000000000 ) ) ;
#3271 = CARTESIAN_POINT ( 'NONE',  ( 16.46437642130999990, 2.740937500800999960, 9.320585551182000827 ) ) ;
#3272 = CARTESIAN_POINT ( 'NONE',  ( 18.59037132503243228, 10.30267188619290408, 1.600077239284419806 ) ) ;
#3273 = EDGE_LOOP ( 'NONE', ( #22901, #1492, #19981 ) ) ;
#3274 = CARTESIAN_POINT ( 'NONE',  ( -22.56945280195751735, 4.659483922790810695, 8.084632350547995117 ) ) ;
#3275 = CARTESIAN_POINT ( 'NONE',  ( 1.923732104253000230, 29.24474039006999959, -1.647538756507999969 ) ) ;
#3276 = CONICAL_SURFACE ( 'NONE', #23355, 9.161549281532000322, 0.02565634000431304615 ) ;
#3277 = CIRCLE ( 'NONE', #6749, 4.000000000000000000 ) ;
#3278 = CARTESIAN_POINT ( 'NONE',  ( 0.000000000000000000, -7.216878364870000340, -12.50000000000000000 ) ) ;
#3279 = PLANE ( 'NONE',  #2319 ) ;
#3280 = ORIENTED_EDGE ( 'NONE', *, *, #6602, .T. ) ;
#3281 = DIRECTION ( 'NONE',  ( 0.000000000000000000, 0.000000000000000000, -1.000000000000000000 ) ) ;
#3282 = CARTESIAN_POINT ( 'NONE',  ( -24.24003052285332416, -12.62002563673716082, 3.141177558950714488 ) ) ;
#3283 = CARTESIAN_POINT ( 'NONE',  ( 16.48520833333332547, -9.094324649508100933, 1.190571260499372785 ) ) ;
#3284 = DIRECTION ( 'NONE',  ( 1.000000000000000000, 0.000000000000000000, 0.000000000000000000 ) ) ;
#3285 = CARTESIAN_POINT ( 'NONE',  ( 14.11337511726693528, -5.197435860462716661, -8.961902679360624902 ) ) ;
#3286 = CARTESIAN_POINT ( 'NONE',  ( -2.164939593608602220, 24.49999999999984368, 3.368873696368141157 ) ) ;
#3287 = CARTESIAN_POINT ( 'NONE',  ( -4.927853318462999788, 12.50793478510998646, 0.4287087720616001296 ) ) ;
#3288 = CARTESIAN_POINT ( 'NONE',  ( 23.99062354302999722, 13.93375672974000068, -0.8660254037843999608 ) ) ;
#3289 = EDGE_LOOP ( 'NONE', ( #18203, #18809 ) ) ;
#3290 = CARTESIAN_POINT ( 'NONE',  ( 61.60588651278290939, 35.51856778792605240, -6.000000000000000000 ) ) ;
#3291 = DIRECTION ( 'NONE',  ( 0.000000000000000000, -1.000000000000000000, -5.996561511235021317E-10 ) ) ;
#3292 = EDGE_LOOP ( 'NONE', ( #8266, #3711, #23634, #7882 ) ) ;
#3293 = EDGE_CURVE ( 'NONE', #959, #15568, #1134, .T. ) ;
#3294 = CARTESIAN_POINT ( 'NONE',  ( -0.7463595094371999750, 23.89665089995999736, -2.539480043651999974 ) ) ;
#3295 = CARTESIAN_POINT ( 'NONE',  ( 2.399999999999999911, 28.00000000000000000, 0.000000000000000000 ) ) ;
#3296 = CARTESIAN_POINT ( 'NONE',  ( 11.36448692216918310, 2.758025466607516130, -12.49997558795211994 ) ) ;
#3297 = FACE_OUTER_BOUND ( 'NONE', #3849, .T. ) ;
#3298 = CARTESIAN_POINT ( 'NONE',  ( -2.434931691670790155, 27.96666666666666856, -0.6543697108981958444 ) ) ;
#3299 = LINE ( 'NONE', #5001, #8636 ) ;
#3300 = ORIENTED_EDGE ( 'NONE', *, *, #7355, .F. ) ;
#3301 = DIRECTION ( 'NONE',  ( 0.000000000000000000, 1.000000000000000000, 0.000000000000000000 ) ) ;
#3302 = VECTOR ( 'NONE', #15662, 1000.000000000000000 ) ;
#3303 = CARTESIAN_POINT ( 'NONE',  ( -1.963534593326285549, 26.23539207552441255, 0.8393142750368668414 ) ) ;
#3304 = CARTESIAN_POINT ( 'NONE',  ( 0.4755391251864483082, 26.25858828695499270, 2.107219116345798948 ) ) ;
#3305 = VERTEX_POINT ( 'NONE', #3389 ) ;
#3306 = EDGE_CURVE ( 'NONE', #3998, #19300, #17276, .T. ) ;
#3307 = CARTESIAN_POINT ( 'NONE',  ( -22.83232346421999992, -9.588805902508001466, 4.859514279198000608 ) ) ;
#3308 = CARTESIAN_POINT ( 'NONE',  ( 20.45333333333332249, -4.631475266059001505, -8.035426097018820712 ) ) ;
#3309 = CARTESIAN_POINT ( 'NONE',  ( 14.54181763333886224, 2.757009540540801940, -9.946943164393594827 ) ) ;
#3310 = CIRCLE ( 'NONE', #5973, 2.000000000000000000 ) ;
#3311 = DIRECTION ( 'NONE',  ( 0.000000000000000000, 1.000000000000000000, 0.000000000000000000 ) ) ;
#3312 = CARTESIAN_POINT ( 'NONE',  ( 18.61948385635999870, 2.167412405366000439, 10.19942539954999994 ) ) ;
#3313 = CARTESIAN_POINT ( 'NONE',  ( 2.095827788178000084, 29.72344142836000103, -0.5546981053674999718 ) ) ;
#3314 = DIRECTION ( 'NONE',  ( -0.7071067811823850136, 0.7071067811898851252, -1.080116767747976029E-06 ) ) ;
#3315 = CARTESIAN_POINT ( 'NONE',  ( 4.156984850324001890, 12.39561475064999385, -2.315346335006999823 ) ) ;
#3316 = VERTEX_POINT ( 'NONE', #10412 ) ;
#3317 = CARTESIAN_POINT ( 'NONE',  ( -1.955724675740084795, 26.26076676662178855, 0.9180910909140133080 ) ) ;
#3318 = VERTEX_POINT ( 'NONE', #23474 ) ;
#3319 = CARTESIAN_POINT ( 'NONE',  ( -6.045495691042000352, 16.31816057295000277, 1.000000020649999932 ) ) ;
#3320 = CIRCLE ( 'NONE', #21858, 1.750000000000000000 ) ;
#3321 = FACE_OUTER_BOUND ( 'NONE', #21911, .T. ) ;
#3322 = EDGE_LOOP ( 'NONE', ( #601, #9624, #5976 ) ) ;
#3323 = B_SPLINE_CURVE_WITH_KNOTS ( 'NONE', 3,
 ( #3247, #17413, #807, #12564, #21882, #14827, #8820, #61, #7100, #3371, #5522, #14490, #8933, #16180, #20301, #22221, #23692, #14604 ),
 .UNSPECIFIED., .F., .F.,
 ( 4, 2, 2, 2, 2, 2, 2, 2, 4 ),
 ( 0.000000000000000000, 0.1250000000000000278, 0.2500000000000000555, 0.3750000000000001110, 0.5000000000000001110, 0.6250000000000001110, 0.7500000000000002220, 0.8750000000000001110, 1.000000000000000000 ),
 .UNSPECIFIED. ) ;
#3324 = EDGE_CURVE ( 'NONE', #8938, #93, #23943, .T. ) ;
#3325 = CARTESIAN_POINT ( 'NONE',  ( -2.899999999999999911, 18.00000000000000000, 0.000000000000000000 ) ) ;
#3326 = CARTESIAN_POINT ( 'NONE',  ( 11.07373617191559845, -11.07537056389462649, -5.816824279993104696 ) ) ;
#3327 = DIRECTION ( 'NONE',  ( 0.000000000000000000, 0.000000000000000000, 1.000000000000000000 ) ) ;
#3328 = ADVANCED_BREP_SHAPE_REPRESENTATION ( '', ( #872, #4390 ), #7088 ) ;
#3329 = CARTESIAN_POINT ( 'NONE',  ( 13.12920410816999883, 3.893241004392999915, 9.759185651010000129 ) ) ;
#3330 = ORIENTED_EDGE ( 'NONE', *, *, #15329, .F. ) ;
#3331 = CARTESIAN_POINT ( 'NONE',  ( 2.899999999999999911, 18.00000000000000000, 0.000000000000000000 ) ) ;
#3332 = CARTESIAN_POINT ( 'NONE',  ( 13.50000000000000000, 7.504433909277588022, 6.535239850074254342 ) ) ;
#3333 = CARTESIAN_POINT ( 'NONE',  ( 0.000000000000000000, 30.00000000000000000, 0.000000000000000000 ) ) ;
#3334 = VECTOR ( 'NONE', #22437, 1000.000000000000000 ) ;
#3335 = ORIENTED_EDGE ( 'NONE', *, *, #21504, .T. ) ;
#3336 = EDGE_CURVE ( 'NONE', #12931, #3365, #10140, .T. ) ;
#3337 = SURFACE_STYLE_FILL_AREA ( #19920 ) ;
#3338 = CARTESIAN_POINT ( 'NONE',  ( 23.20586424138126702, -4.586665969535743237, -9.551222875646683264 ) ) ;
#3339 = AXIS2_PLACEMENT_3D ( 'NONE', #19096, #558, #6018 ) ;
#3340 = CARTESIAN_POINT ( 'NONE',  ( -14.00000000000000000, 5.799910849219894082, 7.344702494732569420 ) ) ;
#3341 = CARTESIAN_POINT ( 'NONE',  ( 17.66124667370037571, -10.36187076387821726, -0.9006624543728345422 ) ) ;
#3342 = CARTESIAN_POINT ( 'NONE',  ( -17.18218939125000233, -9.729142757502000194, -5.298450458072998970 ) ) ;
#3343 = CARTESIAN_POINT ( 'NONE',  ( -2.174612639932000047, 31.01849766815000109, -0.2438152186914000208 ) ) ;
#3344 = B_SPLINE_CURVE_WITH_KNOTS ( 'NONE', 3,
 ( #14337, #11050, #1727, #5363, #9230, #1843, #16608, #9114, #19, #8891, #3551, #9003 ),
 .UNSPECIFIED., .F., .F.,
 ( 4, 1, 1, 1, 1, 2, 2, 4 ),
 ( 0.000000000000000000, 0.2500000000000002220, 0.3750000000000003331, 0.4375000000000003886, 0.4687500000000004441, 0.4843750000000004441, 0.5000000000000004441, 1.000000000000000000 ),
 .UNSPECIFIED. ) ;
#3345 = UNCERTAINTY_MEASURE_WITH_UNIT (LENGTH_MEASURE( 1.000000000000000082E-05 ), #6500, 'distance_accuracy_value', 'NONE');
#3346 = CARTESIAN_POINT ( 'NONE',  ( -15.14859190273999801, -7.578844389069999465, 6.091136938512000221 ) ) ;
#3347 = CARTESIAN_POINT ( 'NONE',  ( 1.707696274334971287, 29.88778704512333206, -1.322457110828678228 ) ) ;
#3348 = VERTEX_POINT ( 'NONE', #1071 ) ;
#3349 = CARTESIAN_POINT ( 'NONE',  ( 11.36448692217191336, 12.20430913916406723, -3.861467675590581017 ) ) ;
#3350 = CARTESIAN_POINT ( 'NONE',  ( 23.25008103265993853, -8.808711889959772279, -5.889380441415137390 ) ) ;
#3351 = CARTESIAN_POINT ( 'NONE',  ( -1.120021599579974714, 23.61859144982829051, -1.799604945664644351 ) ) ;
#3352 = ORIENTED_EDGE ( 'NONE', *, *, #5980, .F. ) ;
#3353 = EDGE_CURVE ( 'NONE', #17972, #2909, #21429, .T. ) ;
#3354 = CYLINDRICAL_SURFACE ( 'NONE', #9131, 1.500000000000000000 ) ;
#3355 = CARTESIAN_POINT ( 'NONE',  ( 4.853323543749686664, 14.55746228791980812, -3.781984119402277855 ) ) ;
#3356 = EDGE_CURVE ( 'NONE', #19694, #7466, #2197, .T. ) ;
#3357 = CIRCLE ( 'NONE', #599, 12.50000000000000178 ) ;
#3358 = CARTESIAN_POINT ( 'NONE',  ( -0.6021973048112005955, 11.45120988776001347, -4.827765333209999454 ) ) ;
#3359 = ORIENTED_EDGE ( 'NONE', *, *, #3772, .T. ) ;
#3360 = CARTESIAN_POINT ( 'NONE',  ( 16.10887625731000128, 5.681759715831000257, 7.231772086132999711 ) ) ;
#3361 = ORIENTED_EDGE ( 'NONE', *, *, #19554, .F. ) ;
#3362 = CARTESIAN_POINT ( 'NONE',  ( 1.785052107064501126, 26.50936796496311132, -1.283493281972921451 ) ) ;
#3363 = VECTOR ( 'NONE', #2471, 1000.000000000000000 ) ;
#3364 = FACE_OUTER_BOUND ( 'NONE', #5541, .T. ) ;
#3365 = VERTEX_POINT ( 'NONE', #5779 ) ;
#3366 = EDGE_CURVE ( 'NONE', #9620, #7062, #596, .T. ) ;
#3367 = DIRECTION ( 'NONE',  ( 0.9996708941621513800, -0.02565352539212875996, 0.000000000000000000 ) ) ;
#3368 = EDGE_CURVE ( 'NONE', #21355, #20086, #9928, .T. ) ;
#3369 = CARTESIAN_POINT ( 'NONE',  ( -19.83169160925000085, -8.995645751853000860, 5.591779661146000002 ) ) ;
#3370 = CARTESIAN_POINT ( 'NONE',  ( -14.94877296625000085, -7.864110397542998676, 5.708624538612000698 ) ) ;
#3371 = CARTESIAN_POINT ( 'NONE',  ( 18.75270833333332376, -1.198188119826038678, -9.152513168516252406 ) ) ;
#3372 = CARTESIAN_POINT ( 'NONE',  ( -23.77841198977664661, 7.775167525423574588, 7.193020863907117146 ) ) ;
#3373 = CARTESIAN_POINT ( 'NONE',  ( -0.1931865607023463827, 26.39289974830605345, 2.197767691045115157 ) ) ;
#3374 = CARTESIAN_POINT ( 'NONE',  ( 0.1690226414553999690, 27.85250240010000056, -2.866097959738999723 ) ) ;
#3375 = CARTESIAN_POINT ( 'NONE',  ( 1.407170236475686842, 30.71340226525985173, -1.638603115233653540 ) ) ;
#3376 = ORIENTED_EDGE ( 'NONE', *, *, #21054, .T. ) ;
#3377 = CARTESIAN_POINT ( 'NONE',  ( -1.595510613210902928, 26.49040384242091761, -3.697633671484740425 ) ) ;
#3378 = DIRECTION ( 'NONE',  ( 0.000000000000000000, -0.8660254037844288266, 0.5000000000000169864 ) ) ;
#3379 = CARTESIAN_POINT ( 'NONE',  ( -1.472309056329999866, 27.63369850838000374, -1.723852419406000092 ) ) ;
#3380 = CARTESIAN_POINT ( 'NONE',  ( 5.836855219999685929, 14.45009295325265697, -1.856713035812031620 ) ) ;
#3381 = CARTESIAN_POINT ( 'NONE',  ( 2.343805879471000164, 25.85187716036000083, -0.7105796827304000640 ) ) ;
#3382 = CONICAL_SURFACE ( 'NONE', #20750, 3.049999825846000157, 0.7853981633972997312 ) ;
#3383 = CARTESIAN_POINT ( 'NONE',  ( 3.731864964225694692, 12.06477785729058283, 3.073113330803231236 ) ) ;
#3384 = ORIENTED_EDGE ( 'NONE', *, *, #16929, .F. ) ;
#3385 = CIRCLE ( 'NONE', #7608, 7.000000000000000000 ) ;
#3386 = CARTESIAN_POINT ( 'NONE',  ( 3.623732334858088322, 12.03139012425049970, -3.204893096957067922 ) ) ;
#3387 = CARTESIAN_POINT ( 'NONE',  ( -10.05747503393159903, 16.19757463933138553, 1.000000000003420819 ) ) ;
#3388 = CIRCLE ( 'NONE', #9163, 12.50000000000000000 ) ;
#3389 = CARTESIAN_POINT ( 'NONE',  ( -3.000000000000000000, 22.00000000000000000, 0.000000000000000000 ) ) ;
#3390 = VERTEX_POINT ( 'NONE', #11242 ) ;
#3391 = CARTESIAN_POINT ( 'NONE',  ( 0.6543697108982381438, 24.23333333333333073, 2.434931691670778608 ) ) ;
#3392 = CARTESIAN_POINT ( 'NONE',  ( -16.21509587121331819, 4.576700897026971582, -7.940391755668851914 ) ) ;
#3393 = CARTESIAN_POINT ( 'NONE',  ( 18.10968892130999919, 7.460570333748000493, 6.290326521484000288 ) ) ;
#3394 = CARTESIAN_POINT ( 'NONE',  ( 18.58888770137535573, 10.31100517592262555, 1.545193600490515573 ) ) ;
#3395 = UNCERTAINTY_MEASURE_WITH_UNIT (LENGTH_MEASURE( 1.000000000000000082E-05 ), #4305, 'distance_accuracy_value', 'NONE');
#3396 = EDGE_LOOP ( 'NONE', ( #12792, #9859, #16166, #20728 ) ) ;
#3397 = CARTESIAN_POINT ( 'NONE',  ( 3.999996093285163035, 28.12756664670878592, 1.519951541579177778 ) ) ;
#3398 = CARTESIAN_POINT ( 'NONE',  ( -0.8605612368241999377, 30.29128581794000041, 1.971086656256000103 ) ) ;
#3399 = FACE_OUTER_BOUND ( 'NONE', #494, .T. ) ;
#3400 = DIRECTION ( 'NONE',  ( 0.000000000000000000, 0.5000000000000169864, -0.8660254037844288266 ) ) ;
#3401 = AXIS2_PLACEMENT_3D ( 'NONE', #12949, #23506, #3178 ) ;
#3402 = VERTEX_POINT ( 'NONE', #5890 ) ;
#3403 = CARTESIAN_POINT ( 'NONE',  ( 0.000000000000000000, 28.00000000000000000, -4.000000000000614619 ) ) ;
#3404 = CARTESIAN_POINT ( 'NONE',  ( 24.37377967401999612, 0.3913942306882999822, 11.36483370893999911 ) ) ;
#3405 = CARTESIAN_POINT ( 'NONE',  ( 0.3272492347489617259, 29.01666666666666572, 2.499999999999996447 ) ) ;
#3406 = AXIS2_PLACEMENT_3D ( 'NONE', #84, #23949, #20675 ) ;
#3407 = LINE ( 'NONE', #3520, #1107 ) ;
#3408 = CARTESIAN_POINT ( 'NONE',  ( -3.748176061208841947, 14.15044768785049101, 4.861384448517857670 ) ) ;
#3409 = CARTESIAN_POINT ( 'NONE',  ( -12.25000000000000000, 12.86886241750721105, -7.894071469735785662 ) ) ;
#3410 = CIRCLE ( 'NONE', #16911, 2.673746900119611247 ) ;
#3411 = CARTESIAN_POINT ( 'NONE',  ( -19.30323503384000361, -9.318276757531000598, 5.904625933860000231 ) ) ;
#3412 = ORIENTED_EDGE ( 'NONE', *, *, #15473, .T. ) ;
#3413 = DIRECTION ( 'NONE',  ( 0.000000000000000000, 0.000000000000000000, -1.000000000000000000 ) ) ;
#3414 = DIRECTION ( 'NONE',  ( -1.000000000000000000, 0.000000000000000000, 0.000000000000000000 ) ) ;
#3415 = ORIENTED_EDGE ( 'NONE', *, *, #13696, .T. ) ;
#3416 = CARTESIAN_POINT ( 'NONE',  ( 2.431246278770999858, 25.97421836118000016, -0.3831752036581999588 ) ) ;
#3417 = DIRECTION ( 'NONE',  ( 1.000000000000000000, 0.000000000000000000, 0.000000000000000000 ) ) ;
#3418 = CARTESIAN_POINT ( 'NONE',  ( 11.92450592358142636, 4.711271677195460583, -12.50004466714985618 ) ) ;
#3419 = AXIS2_PLACEMENT_3D ( 'NONE', #14593, #6732, #12672 ) ;
#3420 = PRESENTATION_LAYER_ASSIGNMENT (  '', '', ( #16148 ) ) ;
#3421 = CARTESIAN_POINT ( 'NONE',  ( 19.24399999999999977, 9.165120680968000144, 0.000000000000000000 ) ) ;
#3422 = CARTESIAN_POINT ( 'NONE',  ( 0.000000000000000000, 20.04999987253367877, 0.000000000000000000 ) ) ;
#3423 = CARTESIAN_POINT ( 'NONE',  ( -2.251038631694548986, 23.88666666666668448, -0.9061425655839590032 ) ) ;
#3424 = VERTEX_POINT ( 'NONE', #9416 ) ;
#3425 = CARTESIAN_POINT ( 'NONE',  ( -0.1529142988638288181, 26.50000000000000355, -2.395123632968240823 ) ) ;
#3426 = DIRECTION ( 'NONE',  ( -0.3292854386466978478, 0.9442304273297127404, 0.000000000000000000 ) ) ;
#3427 = CARTESIAN_POINT ( 'NONE',  ( 11.00000000000000000, -10.59999999999999964, 0.000000000000000000 ) ) ;
#3428 = EDGE_LOOP ( 'NONE', ( #8749, #10212 ) ) ;
#3429 = CARTESIAN_POINT ( 'NONE',  ( -10.64917158021815879, 15.44101125622223947, -1.507928438456294096 ) ) ;
#3430 = CARTESIAN_POINT ( 'NONE',  ( 0.01686421794022999882, 25.08949700035999797, -2.144542314183000009 ) ) ;
#3431 = CARTESIAN_POINT ( 'NONE',  ( 14.44670397028254172, -0.5670727829898102312, -10.31211031097369002 ) ) ;
#3432 = DIRECTION ( 'NONE',  ( 0.000000000000000000, 1.000000000000000000, 0.000000000000000000 ) ) ;
#3433 = CARTESIAN_POINT ( 'NONE',  ( 20.82204741195999986, -10.17246175326000035, 4.719653495980000280 ) ) ;
#3434 = ADVANCED_FACE ( 'NONE', ( #9178 ), #23470, .T. ) ;
#3435 = CARTESIAN_POINT ( 'NONE',  ( -1.875937833822000078, 30.94419248354000374, 0.8416011999412000844 ) ) ;
#3436 = B_SPLINE_CURVE_WITH_KNOTS ( 'NONE', 3,
 ( #14345, #2723, #15900, #16016, #6467, #19803, #15654, #13976 ),
 .UNSPECIFIED., .F., .F.,
 ( 4, 2, 2, 4 ),
 ( 0.000000000000000000, 0.2499999999999999445, 0.4999999999999998890, 1.000000000000000000 ),
 .UNSPECIFIED. ) ;
#3437 = CARTESIAN_POINT ( 'NONE',  ( 4.701265373510000956, 12.59995792350999189, -1.092434317656999054 ) ) ;
#3438 = CARTESIAN_POINT ( 'NONE',  ( -22.11059587121331305, -8.072587028924724351, -4.652893487818362317 ) ) ;
#3439 = ORIENTED_EDGE ( 'NONE', *, *, #3306, .F. ) ;
#3440 = DIRECTION ( 'NONE',  ( 1.000000000000000000, 0.000000000000000000, 0.000000000000000000 ) ) ;
#3441 = ORIENTED_EDGE ( 'NONE', *, *, #1584, .T. ) ;
#3442 = CONICAL_SURFACE ( 'NONE', #15006, 2.849999993810000021, 0.7853981633972997312 ) ;
#3443 = CARTESIAN_POINT ( 'NONE',  ( -0.3418248460082276563, 30.21683089135267508, -2.592948918868650754 ) ) ;
#3444 = CARTESIAN_POINT ( 'NONE',  ( 16.59858333333331970, -8.860506003517219398, -2.381064488431900994 ) ) ;
#3445 = EDGE_CURVE ( 'NONE', #16168, #23400, #13162, .T. ) ;
#3446 = CARTESIAN_POINT ( 'NONE',  ( 0.000000000000000000, -10.00000000000000000, 0.000000000000000000 ) ) ;
#3447 = AXIS2_PLACEMENT_3D ( 'NONE', #1825, #10807, #5233 ) ;
#3448 = CARTESIAN_POINT ( 'NONE',  ( 18.26830054543999893, 10.39455046184000153, -3.947462618599999917 ) ) ;
#3449 = ORIENTED_EDGE ( 'NONE', *, *, #10282, .T. ) ;
#3450 = CARTESIAN_POINT ( 'NONE',  ( -9.290830065846000352, -6.196630076247999774, -13.51516600793999956 ) ) ;
#3451 = AXIS2_PLACEMENT_3D ( 'NONE', #3986, #17426, #10160 ) ;
#3452 = CARTESIAN_POINT ( 'NONE',  ( 13.50000000000000000, 9.141558265356509949, -2.348328869579741518 ) ) ;
#3453 = CARTESIAN_POINT ( 'NONE',  ( -14.41332674684390369, -12.63239273137551777, -3.119888754839689415 ) ) ;
#3454 = EDGE_LOOP ( 'NONE', ( #12677, #20314, #8681, #5924, #9418 ) ) ;
#3455 =( NAMED_UNIT ( * ) SI_UNIT ( $, .STERADIAN. ) SOLID_ANGLE_UNIT ( ) );
#3456 = CARTESIAN_POINT ( 'NONE',  ( 20.64679523879173928, -1.188210788644911142, 10.46129133059315564 ) ) ;
#3457 = DIRECTION ( 'NONE',  ( 0.000000000000000000, 0.000000000000000000, -1.000000000000000000 ) ) ;
#3458 = CARTESIAN_POINT ( 'NONE',  ( 16.10203026881945121, -5.935666563581813548, -8.493690021681720381 ) ) ;
#3459 = CIRCLE ( 'NONE', #22010, 3.000000000000002665 ) ;
#3460 = EDGE_CURVE ( 'NONE', #4661, #14273, #11305, .T. ) ;
#3461 = CARTESIAN_POINT ( 'NONE',  ( -0.3635937247009000117, 28.79408723144999627, 2.231225001579999923 ) ) ;
#3462 = TOROIDAL_SURFACE ( 'NONE', #4609, 10.50000000000000000, 0.1000000000000000056 ) ;
#3463 = CARTESIAN_POINT ( 'NONE',  ( -14.53920085882999835, -1.325901587985999885, -9.615240848067001522 ) ) ;
#3464 = CARTESIAN_POINT ( 'NONE',  ( 2.067250320083055648, 29.84154813460735056, -0.6328137310853092501 ) ) ;
#3465 = ORIENTED_EDGE ( 'NONE', *, *, #1684, .T. ) ;
#3466 = CARTESIAN_POINT ( 'NONE',  ( 21.20719740893701655, -10.32741046810345509, 2.129377785346741714 ) ) ;
#3467 = DIRECTION ( 'NONE',  ( 0.8206518289197729521, -0.5714285394435874021, -4.207939614820930173E-10 ) ) ;
#3468 = ORIENTED_EDGE ( 'NONE', *, *, #23142, .T. ) ;
#3469 = CARTESIAN_POINT ( 'NONE',  ( 12.52688711657000020, 6.216878364870000340, 12.50000000000000000 ) ) ;
#3470 = CARTESIAN_POINT ( 'NONE',  ( 4.855310581006569315, 14.54728511032672422, -3.783400810746735399 ) ) ;
#3471 = ADVANCED_FACE ( 'NONE', ( #10884 ), #8404, .T. ) ;
#3472 = CARTESIAN_POINT ( 'NONE',  ( 1.394400747533001361, 11.57446794508000742, -4.613298798923998412 ) ) ;
#3473 = ORIENTED_EDGE ( 'NONE', *, *, #16950, .F. ) ;
#3474 = CIRCLE ( 'NONE', #8903, 2.000000000000000000 ) ;
#3475 = CARTESIAN_POINT ( 'NONE',  ( 12.50897833293000083, -6.466896515026999914, -12.35565195369999891 ) ) ;
#3476 = ORIENTED_EDGE ( 'NONE', *, *, #10113, .F. ) ;
#3477 = VECTOR ( 'NONE', #17700, 1000.000000000000000 ) ;
#3478 = DIRECTION ( 'NONE',  ( 1.000000000000000000, 0.000000000000000000, 0.000000000000000000 ) ) ;
#3479 = EDGE_CURVE ( 'NONE', #20864, #20904, #2580, .T. ) ;
#3480 = CARTESIAN_POINT ( 'NONE',  ( -0.6543697108981931798, 29.76666666666666217, 2.434931691670791043 ) ) ;
#3481 = ORIENTED_EDGE ( 'NONE', *, *, #4962, .F. ) ;
#3482 = CARTESIAN_POINT ( 'NONE',  ( -10.04701370327999932, 16.31160201366999729, -1.000000000000000000 ) ) ;
#3483 = CARTESIAN_POINT ( 'NONE',  ( -24.11553951883000124, 3.250485078146000184, 9.656343706050000364 ) ) ;
#3484 = ADVANCED_FACE ( 'NONE', ( #23947 ), #8790, .F. ) ;
#3485 = CARTESIAN_POINT ( 'NONE',  ( 12.52688711657000020, -7.716878364870000340, -11.63397459621999985 ) ) ;
#3486 = CARTESIAN_POINT ( 'NONE',  ( -6.294318966394004455, 15.05816953584999851, -3.444806853728002327 ) ) ;
#3487 = ADVANCED_FACE ( 'NONE', ( #312 ), #22019, .T. ) ;
#3488 = CARTESIAN_POINT ( 'NONE',  ( -24.29311450473293021, 5.407626218985153166, -9.123098698783515204 ) ) ;
#3489 = CARTESIAN_POINT ( 'NONE',  ( 1.740441092190665895, 27.32044006443200601, 1.359758610450851446 ) ) ;
#3490 = CARTESIAN_POINT ( 'NONE',  ( 1.182158213329999930, 29.12000240010000240, 2.320116128650000054 ) ) ;
#3491 = CIRCLE ( 'NONE', #17003, 2.899999999999999911 ) ;
#3492 = CARTESIAN_POINT ( 'NONE',  ( 2.021074183709790528, 30.64977378284504539, -0.7618599147945216421 ) ) ;
#3493 = VERTEX_POINT ( 'NONE', #13517 ) ;
#3494 = CARTESIAN_POINT ( 'NONE',  ( -1.839173991642404138, 26.50000000000000355, -3.556954554355651776 ) ) ;
#3495 = DIRECTION ( 'NONE',  ( 0.000000000000000000, 1.000000000000000000, 0.000000000000000000 ) ) ;
#3496 = CARTESIAN_POINT ( 'NONE',  ( 1.629375854237163912, 24.77111710846513404, 1.370482674755798769 ) ) ;
#3497 = CARTESIAN_POINT ( 'NONE',  ( -1.800284464616000113, 27.67364211382000150, 1.419229835182000077 ) ) ;
#3498 = EDGE_CURVE ( 'NONE', #14786, #2047, #2378, .T. ) ;
#3499 = VECTOR ( 'NONE', #9426, 1000.000000000000000 ) ;
#3500 = DIRECTION ( 'NONE',  ( -1.000000000000000000, 0.000000000000000000, 0.000000000000000000 ) ) ;
#3501 = ORIENTED_EDGE ( 'NONE', *, *, #10008, .F. ) ;
#3502 = CARTESIAN_POINT ( 'NONE',  ( -4.040251331918567779, 12.16185153434827093, -2.666099664634059341 ) ) ;
#3503 = CARTESIAN_POINT ( 'NONE',  ( 24.13033325080091274, -0.1217589085045256286, -9.517347760093475273 ) ) ;
#3504 = CARTESIAN_POINT ( 'NONE',  ( -0.6743924145742135057, 30.66853591686814440, -2.175867686628469855 ) ) ;
#3505 = ORIENTED_EDGE ( 'NONE', *, *, #15253, .F. ) ;
#3506 = CARTESIAN_POINT ( 'NONE',  ( 0.000000000000000000, 9.000000000000000000, 0.000000000000000000 ) ) ;
#3507 = DIRECTION ( 'NONE',  ( 0.7071067811865465735, 0.7071067811865465735, 5.135208691342337292E-08 ) ) ;
#3508 = B_SPLINE_CURVE_WITH_KNOTS ( 'NONE', 3,
 ( #15476, #17176, #21177, #2651, #19237, #22860, #15590, #21052, #13777, #22503, #11982, #4104, #5913, #11503, #17915, #8468, #8587, #17669 ),
 .UNSPECIFIED., .F., .F.,
 ( 4, 2, 2, 2, 2, 2, 2, 2, 4 ),
 ( 0.000000000000000000, 0.1250000000000000278, 0.2500000000000000555, 0.3750000000000001110, 0.5000000000000001110, 0.6250000000000001110, 0.7500000000000002220, 0.8750000000000002220, 1.000000000000000000 ),
 .UNSPECIFIED. ) ;
#3509 = CARTESIAN_POINT ( 'NONE',  ( 11.74781392131000146, -7.601052271439000307, -5.849495945765999849 ) ) ;
#3510 = CARTESIAN_POINT ( 'NONE',  ( 18.81959018942939466, 6.044305804050750019, 8.501725326887493495 ) ) ;
#3511 = ADVANCED_FACE ( 'NONE', ( #17034 ), #4827, .F. ) ;
#3512 = DIRECTION ( 'NONE',  ( 0.000000000000000000, 0.000000000000000000, -1.000000000000000000 ) ) ;
#3513 = CARTESIAN_POINT ( 'NONE',  ( 1.341975064934000095, 29.62948861319000216, 1.680729365189000069 ) ) ;
#3514 = CARTESIAN_POINT ( 'NONE',  ( 17.08796080085999947, 1.565451709191000074, 11.28839175225999902 ) ) ;
#3515 = CARTESIAN_POINT ( 'NONE',  ( 13.50000000000000355, -9.490788312992085807, -1.343451305609774993 ) ) ;
#3516 = EDGE_LOOP ( 'NONE', ( #21764, #17810, #18464, #16532, #2678, #6284, #6194 ) ) ;
#3517 = CARTESIAN_POINT ( 'NONE',  ( -23.99212502904700983, 13.39645431917582030, 1.796660477929257427 ) ) ;
#3518 = CARTESIAN_POINT ( 'NONE',  ( 21.18689583523000053, -11.25120934773000059, 0.8723638986538000406 ) ) ;
#3519 = CARTESIAN_POINT ( 'NONE',  ( -3.100000000000000089, 15.00000000000000000, 0.000000000000000000 ) ) ;
#3520 = CARTESIAN_POINT ( 'NONE',  ( -4.563746053395999702, 28.00000000000000000, 4.080056528100000079 ) ) ;
#3521 = DIRECTION ( 'NONE',  ( 1.000000000000000000, 0.000000000000000000, 0.000000000000000000 ) ) ;
#3522 = CARTESIAN_POINT ( 'NONE',  ( 1.673502882357000177, 11.64651242530998410, 4.674820881733997346 ) ) ;
#3523 = CARTESIAN_POINT ( 'NONE',  ( -1.633064903454896966, 29.31302280117960990, -1.413517025400313321 ) ) ;
#3524 = CARTESIAN_POINT ( 'NONE',  ( -1.767766952966000060, 30.50000000000000000, 1.767766952966000060 ) ) ;
#3525 = EDGE_LOOP ( 'NONE', ( #17576, #3926, #8622, #8440, #2866, #17469, #7430 ) ) ;
#3526 = ADVANCED_FACE ( 'NONE', ( #549 ), #14100, .F. ) ;
#3527 = CARTESIAN_POINT ( 'NONE',  ( 2.099577540571663015, 23.85573745231591403, 1.106133451035238524 ) ) ;
#3528 = VERTEX_POINT ( 'NONE', #2624 ) ;
#3529 = CARTESIAN_POINT ( 'NONE',  ( -0.6391230356295000137, 23.90547497936000099, 2.064599356847000244 ) ) ;
#3530 = CARTESIAN_POINT ( 'NONE',  ( 6.598144805745005392, 13.50878560842000020, 0.7964734107506996619 ) ) ;
#3531 = CARTESIAN_POINT ( 'NONE',  ( 11.97297107870701893, 4.846971342257544002, -12.50004942866563340 ) ) ;
#3532 = CARTESIAN_POINT ( 'NONE',  ( 1.709999999999999964, 12.37689379448999993, 0.3720215047547999476 ) ) ;
#3533 = CARTESIAN_POINT ( 'NONE',  ( 13.50000000000000355, -0.4765265073848649058, 10.29322485242600571 ) ) ;
#3534 = EDGE_LOOP ( 'NONE', ( #15704, #13656, #6150, #14286 ) ) ;
#3535 = CARTESIAN_POINT ( 'NONE',  ( -16.16424364259000157, 4.823843515939000071, -8.474820356344999084 ) ) ;
#3536 = VECTOR ( 'NONE', #7475, 1000.000000000000114 ) ;
#3537 = CARTESIAN_POINT ( 'NONE',  ( 0.000000000000000000, 19.00000000000000000, 0.000000000000000000 ) ) ;
#3538 = CARTESIAN_POINT ( 'NONE',  ( -4.000000000000000000, 24.50000000000000000, 0.000000000000000000 ) ) ;
#3539 = ORIENTED_EDGE ( 'NONE', *, *, #12093, .F. ) ;
#3540 = CARTESIAN_POINT ( 'NONE',  ( 0.000000000000000000, 30.00000000000000000, 0.000000000000000000 ) ) ;
#3541 = CARTESIAN_POINT ( 'NONE',  ( -1.946458991525999993, 25.34566145796000214, 0.9003574723619000020 ) ) ;
#3542 = CARTESIAN_POINT ( 'NONE',  ( 14.43179268012507954, -1.084526859950961875, -10.26172237758129846 ) ) ;
#3543 = CARTESIAN_POINT ( 'NONE',  ( 0.000000000000000000, 22.00000000000000000, 0.000000000000000000 ) ) ;
#3544 = CARTESIAN_POINT ( 'NONE',  ( 20.01400882793000235, 5.003195029065000021, -10.01125156252000004 ) ) ;
#3545 = CARTESIAN_POINT ( 'NONE',  ( 0.000000000000000000, 28.15000000000000213, 0.000000000000000000 ) ) ;
#3546 = CARTESIAN_POINT ( 'NONE',  ( 13.69548965135293450, 8.444355585795914720, -3.174683004369278194 ) ) ;
#3547 = CARTESIAN_POINT ( 'NONE',  ( -4.749999884653000493, 20.09999988465641252, 5.093549627072000020E-08 ) ) ;
#3548 = FILL_AREA_STYLE ('',( #20140 ) ) ;
#3549 = ORIENTED_EDGE ( 'NONE', *, *, #5216, .F. ) ;
#3550 = CARTESIAN_POINT ( 'NONE',  ( -14.89767593716247163, -8.438677071178334543, -3.297102474276865092 ) ) ;
#3551 = CARTESIAN_POINT ( 'NONE',  ( 24.50000000000000711, -9.325532229573614273, 5.118943956174335952 ) ) ;
#3552 = EDGE_LOOP ( 'NONE', ( #5007, #17455, #1130, #8586, #15007, #13159 ) ) ;
#3553 = CARTESIAN_POINT ( 'NONE',  ( 19.51605026741271232, -1.735679401533887001, 9.439139126610488262 ) ) ;
#3554 = CARTESIAN_POINT ( 'NONE',  ( 1.803851175814259244, 30.74302359554534192, -1.387995464745191310 ) ) ;
#3555 = LINE ( 'NONE', #16264, #18147 ) ;
#3556 = CARTESIAN_POINT ( 'NONE',  ( 15.23446458303000028, -6.520685359936000403, 8.903299142152000911 ) ) ;
#3557 = CARTESIAN_POINT ( 'NONE',  ( -14.30710121467889273, 1.268344841054370065, 10.26973291966113599 ) ) ;
#3558 = EDGE_CURVE ( 'NONE', #11075, #18791, #22953, .T. ) ;
#3559 = CARTESIAN_POINT ( 'NONE',  ( 1.450871306011999984, 27.86506359723999893, 1.996953125041000199 ) ) ;
#3560 = VERTEX_POINT ( 'NONE', #6499 ) ;
#3561 = CARTESIAN_POINT ( 'NONE',  ( -8.917480899178999110, 13.20694165471999959, -6.150971466210000571 ) ) ;
#3562 = CARTESIAN_POINT ( 'NONE',  ( 0.000000000000000000, 29.85000000000000142, 0.000000000000000000 ) ) ;
#3563 = CARTESIAN_POINT ( 'NONE',  ( -14.25243324638999809, -6.216878364870000340, 12.50000000000000000 ) ) ;
#3564 = ORIENTED_EDGE ( 'NONE', *, *, #20949, .T. ) ;
#3565 = CARTESIAN_POINT ( 'NONE',  ( 22.85288920654172173, -10.53285308750527705, 1.051356703202095844 ) ) ;
#3566 = CARTESIAN_POINT ( 'NONE',  ( 4.724999999999999645, 14.90000000000000036, 0.000000000000000000 ) ) ;
#3567 = CARTESIAN_POINT ( 'NONE',  ( 15.97156973469264152, -9.031727242954262991, -5.071998056861781734 ) ) ;
#3568 = CARTESIAN_POINT ( 'NONE',  ( -17.72417933634999798, -2.118794415358999927, 10.88897014444000177 ) ) ;
#3569 = AXIS2_PLACEMENT_3D ( 'NONE', #19879, #12610, #17944 ) ;
#3570 = CARTESIAN_POINT ( 'NONE',  ( -2.180465314960999823, 31.04811387923000154, 0.5967716603282000598 ) ) ;
#3571 = CARTESIAN_POINT ( 'NONE',  ( -3.999709959627196110, 28.03198827073818578, -0.7544996412928929308 ) ) ;
#3572 = CARTESIAN_POINT ( 'NONE',  ( 2.122511661976075548, 29.82749129234522556, -0.4006784551261859395 ) ) ;
#3573 = ORIENTED_EDGE ( 'NONE', *, *, #18548, .F. ) ;
#3574 = CARTESIAN_POINT ( 'NONE',  ( -1.613915809855000161, 25.52668260664000144, 1.467707619367000227 ) ) ;
#3575 = CARTESIAN_POINT ( 'NONE',  ( 21.12207725794927526, -9.259445203091740240, 5.038593002177021773 ) ) ;
#3576 = CARTESIAN_POINT ( 'NONE',  ( -0.9863764412085774813, 23.62386489563331082, -1.881032207583069216 ) ) ;
#3577 = CIRCLE ( 'NONE', #21362, 3.100000000000000089 ) ;
#3578 = ORIENTED_EDGE ( 'NONE', *, *, #5131, .T. ) ;
#3579 = CARTESIAN_POINT ( 'NONE',  ( 13.21250000000000036, 0.000000000000000000, 0.000000000000000000 ) ) ;
#3580 = CARTESIAN_POINT ( 'NONE',  ( 4.871792852526525053, 14.47489112828897362, -3.795289058065452803 ) ) ;
#3581 = CARTESIAN_POINT ( 'NONE',  ( -2.718451692004000275, 11.82335083566999323, -3.948280308763997493 ) ) ;
#3582 = ORIENTED_EDGE ( 'NONE', *, *, #12006, .F. ) ;
#3583 = EDGE_CURVE ( 'NONE', #2909, #5518, #5506, .T. ) ;
#3584 = CARTESIAN_POINT ( 'NONE',  ( 11.39231375731000107, -8.729484032481000355, -2.472142458034000345 ) ) ;
#3585 = ORIENTED_EDGE ( 'NONE', *, *, #23747, .F. ) ;
#3586 = CIRCLE ( 'NONE', #10935, 12.50000000000000178 ) ;
#3587 = CARTESIAN_POINT ( 'NONE',  ( 61.60588651278290939, 37.01856778792605240, -6.000000000000000000 ) ) ;
#3588 = ITEM_DEFINED_TRANSFORMATION ( 'NONE', 'NONE', #14440,  #4390 ) ;
#3589 = CARTESIAN_POINT ( 'NONE',  ( 2.399999988617999680, 26.49999998861800066, 6.349992443878999481E-08 ) ) ;
#3590 = VERTEX_POINT ( 'NONE', #19711 ) ;
#3591 = DIRECTION ( 'NONE',  ( 0.000000000000000000, 0.5000000000000169864, -0.8660254037844288266 ) ) ;
#3592 = CARTESIAN_POINT ( 'NONE',  ( -20.42204576454999909, 0.9856272077188000802, 10.04066030219000005 ) ) ;
#3593 = EDGE_CURVE ( 'NONE', #17322, #5263, #2994, .T. ) ;
#3594 = CARTESIAN_POINT ( 'NONE',  ( -16.57381575000999874, -9.759477557600000353, -0.2595777249469000125 ) ) ;
#3595 = CARTESIAN_POINT ( 'NONE',  ( -5.431150319964994644, 14.88403208498999142, -3.316913632744003415 ) ) ;
#3596 = CARTESIAN_POINT ( 'NONE',  ( -22.28577469641619402, 9.959647916863344719, -3.842436443305321081 ) ) ;
#3597 = CARTESIAN_POINT ( 'NONE',  ( 2.036279486417807316, 27.45294582375450787, -0.8150601855909705984 ) ) ;
#3598 = DIRECTION ( 'NONE',  ( -1.000000000000000000, 0.000000000000000000, 0.000000000000000000 ) ) ;
#3599 = CARTESIAN_POINT ( 'NONE',  ( 1.686548823153775745, 30.68970166146306511, -1.349673947955718711 ) ) ;
#3600 = ORIENTED_EDGE ( 'NONE', *, *, #10443, .F. ) ;
#3601 = CARTESIAN_POINT ( 'NONE',  ( 23.75578739169031550, -4.482660184358483235, 8.204279979722965521 ) ) ;
#3602 = DIRECTION ( 'NONE',  ( 0.000000000000000000, -1.000000000000000000, 0.000000000000000000 ) ) ;
#3603 = CARTESIAN_POINT ( 'NONE',  ( 13.71789754803960193, 2.629260093309664814, -8.685948811178583640 ) ) ;
#3604 = EDGE_CURVE ( 'NONE', #1114, #12621, #21520, .T. ) ;
#3605 = CARTESIAN_POINT ( 'NONE',  ( 1.981708497821000226, 26.53437716036000182, 1.439795436514999860 ) ) ;
#3606 = CARTESIAN_POINT ( 'NONE',  ( 3.022862379614798645, 11.86775895167101247, 3.763016671309872496 ) ) ;
#3607 = EDGE_LOOP ( 'NONE', ( #874, #13520, #23613, #5720, #6594, #11648 ) ) ;
#3608 = EDGE_CURVE ( 'NONE', #15241, #18990, #17892, .T. ) ;
#3609 = CARTESIAN_POINT ( 'NONE',  ( -3.943681128674290992, 12.13065354962336428, -2.803234342281037961 ) ) ;
#3610 = CARTESIAN_POINT ( 'NONE',  ( -10.30414807049024972, 15.71393056377423036, 1.198114258386445696 ) ) ;
#3611 = CARTESIAN_POINT ( 'NONE',  ( -2.273481569363994925, 30.02225594647815043, -0.1432571156271773005 ) ) ;
#3612 = ORIENTED_EDGE ( 'NONE', *, *, #16285, .T. ) ;
#3613 = CARTESIAN_POINT ( 'NONE',  ( 24.00034722001000276, -7.216970193741999218, 11.92259671338999993 ) ) ;
#3614 = CARTESIAN_POINT ( 'NONE',  ( -18.13088126894000141, 1.446686056264999920E-14, 0.000000000000000000 ) ) ;
#3615 = LINE ( 'NONE', #14654, #10343 ) ;
#3616 = CARTESIAN_POINT ( 'NONE',  ( 16.38112658530999610, 10.11489150981000051, 1.477102707085000022 ) ) ;
#3617 = CARTESIAN_POINT ( 'NONE',  ( 18.52789202429464410, 10.40670619203928915, -0.6213187097667132175 ) ) ;
#3618 = EDGE_CURVE ( 'NONE', #5775, #12558, #17583, .T. ) ;
#3619 = CARTESIAN_POINT ( 'NONE',  ( 1.536366799937295413, 29.31753006952332896, 1.999167105995444338 ) ) ;
#3620 = CARTESIAN_POINT ( 'NONE',  ( -0.7039221594073999944, 28.80840715711999778, 2.125142508213000436 ) ) ;
#3621 = CARTESIAN_POINT ( 'NONE',  ( -12.49883338062999805, 6.877492854395000244, -5.798745594989999752 ) ) ;
#3622 = CARTESIAN_POINT ( 'NONE',  ( 13.49999999999999645, -8.661498127773935352, -3.738203993960828253 ) ) ;
#3623 = ORIENTED_EDGE ( 'NONE', *, *, #11153, .T. ) ;
#3624 = CIRCLE ( 'NONE', #5553, 3.000000000000000000 ) ;
#3625 = FACE_OUTER_BOUND ( 'NONE', #1667, .T. ) ;
#3626 = CARTESIAN_POINT ( 'NONE',  ( 18.94427387461000123, -0.06533020399979999615, 10.75972831271999830 ) ) ;
#3627 = CARTESIAN_POINT ( 'NONE',  ( -24.20872234573575099, 9.568575771055293444, 3.051701187166265594 ) ) ;
#3628 = CARTESIAN_POINT ( 'NONE',  ( 13.94611192983668246, -9.250779629793038694, -4.651112269942151656 ) ) ;
#3629 = DIRECTION ( 'NONE',  ( 1.000000000000000000, 0.000000000000000000, 0.000000000000000000 ) ) ;
#3630 = CARTESIAN_POINT ( 'NONE',  ( -12.25000000000000000, 6.613190111079999767, -13.46349570337000046 ) ) ;
#3631 = CARTESIAN_POINT ( 'NONE',  ( -1.635465687292884773, 29.31323759626713255, -1.410743754062205646 ) ) ;
#3632 = CARTESIAN_POINT ( 'NONE',  ( -21.97658776632000155, 10.22865322212999928, -4.322346676424000833 ) ) ;
#3633 = VERTEX_POINT ( 'NONE', #6978 ) ;
#3634 = DIRECTION ( 'NONE',  ( 0.000000000000000000, 1.000000000000000000, 0.000000000000000000 ) ) ;
#3635 = ORIENTED_EDGE ( 'NONE', *, *, #15775, .F. ) ;
#3636 = EDGE_CURVE ( 'NONE', #12346, #1991, #18352, .T. ) ;
#3637 = DIRECTION ( 'NONE',  ( 0.000000000000000000, 0.000000000000000000, -1.000000000000000000 ) ) ;
#3638 = CARTESIAN_POINT ( 'NONE',  ( 11.45478115325884083, 3.141659414319641463, -12.49993290927501199 ) ) ;
#3639 = EDGE_CURVE ( 'NONE', #23059, #12621, #11389, .T. ) ;
#3640 = CARTESIAN_POINT ( 'NONE',  ( -1.802851389305008434, 26.49891402983596222, 1.731858503842447217 ) ) ;
#3641 = CARTESIAN_POINT ( 'NONE',  ( 23.99478584076000232, -13.93375672974000068, -0.6736217020456000126 ) ) ;
#3642 = CARTESIAN_POINT ( 'NONE',  ( 18.05287674931000197, 3.913226583351999910, -10.03953908883999979 ) ) ;
#3643 = AXIS2_PLACEMENT_3D ( 'NONE', #10921, #14771, #7388 ) ;
#3644 = ORIENTED_EDGE ( 'NONE', *, *, #8463, .T. ) ;
#3645 = CARTESIAN_POINT ( 'NONE',  ( -13.32041877100999905, -7.827390682981001824, 5.681961735881999154 ) ) ;
#3646 = CARTESIAN_POINT ( 'NONE',  ( 4.000000000000000888, 29.94682129341588350, 0.9440428258623109192 ) ) ;
#3647 = DIRECTION ( 'NONE',  ( -1.000000000000000000, 0.000000000000000000, 0.000000000000000000 ) ) ;
#3648 = ORIENTED_EDGE ( 'NONE', *, *, #12504, .F. ) ;
#3649 = ADVANCED_FACE ( 'NONE', ( #1538 ), #19826, .F. ) ;
#3650 = DIRECTION ( 'NONE',  ( -1.000000000000000000, 0.000000000000000000, 2.461955262174999944E-13 ) ) ;
#3651 = EDGE_CURVE ( 'NONE', #9820, #21250, #4659, .T. ) ;
#3652 = CARTESIAN_POINT ( 'NONE',  ( 2.246634820853000036, 25.60312647565999811, -0.3244181043566000122 ) ) ;
#3653 = CARTESIAN_POINT ( 'NONE',  ( 14.53584632513973851, 2.541295010820454614, -10.00545943804216620 ) ) ;
#3654 = CARTESIAN_POINT ( 'NONE',  ( -18.59597087121333558, -9.148490976324819002, -1.197661616099367166 ) ) ;
#3655 = CARTESIAN_POINT ( 'NONE',  ( 23.64802272119000293, -0.2661318661629999971, -11.28844956766999985 ) ) ;
#3656 = CARTESIAN_POINT ( 'NONE',  ( -2.214826247177999807, 30.81482155776999932, 0.5323604184908000692 ) ) ;
#3657 = CARTESIAN_POINT ( 'NONE',  ( 13.61354498824686843, 7.183912508121929719, -5.456131416217646191 ) ) ;
#3658 = CARTESIAN_POINT ( 'NONE',  ( -2.712275836624000291, 11.98432359369998856, -3.994273073785000072 ) ) ;
#3659 = CARTESIAN_POINT ( 'NONE',  ( -21.39255420454665213, 9.220256816434664771, -1.206801847291320229 ) ) ;
#3660 = ORIENTED_EDGE ( 'NONE', *, *, #15591, .T. ) ;
#3661 = CARTESIAN_POINT ( 'NONE',  ( 0.000000000000000000, 29.85000000000000142, 0.000000000000000000 ) ) ;
#3662 = EDGE_LOOP ( 'NONE', ( #11373, #8035, #6815, #21382, #13079, #9124, #18751, #10439 ) ) ;
#3663 = DIRECTION ( 'NONE',  ( 0.000000000000000000, -1.000000000000000000, 0.000000000000000000 ) ) ;
#3664 = CARTESIAN_POINT ( 'NONE',  ( 11.29022434644324235, -12.01543594605075782, -4.188602139406581770 ) ) ;
#3665 = DIRECTION ( 'NONE',  ( -1.000000000000000000, 0.000000000000000000, 0.000000000000000000 ) ) ;
#3666 = VECTOR ( 'NONE', #5384, 999.9999999999998863 ) ;
#3667 = CARTESIAN_POINT ( 'NONE',  ( 13.39612630362000090, -0.4383194471242999879, 10.97614716848999983 ) ) ;
#3668 = FACE_OUTER_BOUND ( 'NONE', #10223, .T. ) ;
#3669 = CARTESIAN_POINT ( 'NONE',  ( 2.826365205286999860, 27.75169433610000169, 0.5047246425490000687 ) ) ;
#3670 = ORIENTED_EDGE ( 'NONE', *, *, #9828, .F. ) ;
#3671 = VECTOR ( 'NONE', #20716, 1000.000000000000114 ) ;
#3672 = CARTESIAN_POINT ( 'NONE',  ( -9.792568638769999723, -15.07240962404999962, 2.103107733322999717 ) ) ;
#3673 = CARTESIAN_POINT ( 'NONE',  ( -0.4421657205835797244, 6.791814712419944833, -1.694527932936234604 ) ) ;
#3674 = DIRECTION ( 'NONE',  ( 0.1400000000000034828, 0.9901515035589245617, 0.000000000000000000 ) ) ;
#3675 = ORIENTED_EDGE ( 'NONE', *, *, #11768, .T. ) ;
#3676 = CARTESIAN_POINT ( 'NONE',  ( -4.927443545268737068, 15.82417552330234223, -3.638606983025983510 ) ) ;
#3677 = CARTESIAN_POINT ( 'NONE',  ( 20.20557644524101804, 10.39545583923814753, 1.631852776342430866 ) ) ;
#3678 = CARTESIAN_POINT ( 'NONE',  ( 24.28255857085268943, 8.769700062105057370, -9.810433925293667201 ) ) ;
#3679 = CARTESIAN_POINT ( 'NONE',  ( 16.11492084001121228, -5.561606119988664609, -8.744802779703126916 ) ) ;
#3680 = CARTESIAN_POINT ( 'NONE',  ( -15.34151452278999983, -5.012687067889999959, -9.822839049446999482 ) ) ;
#3681 = CARTESIAN_POINT ( 'NONE',  ( -1.090723536193999976, 30.35272267939000201, 2.073606040276000151 ) ) ;
#3682 = AXIS2_PLACEMENT_3D ( 'NONE', #18630, #7599, #7130 ) ;
#3683 = CARTESIAN_POINT ( 'NONE',  ( -3.999996093277206732, 28.12756664670158457, -1.519951541552794883 ) ) ;
#3684 = CARTESIAN_POINT ( 'NONE',  ( 1.381408399707872992, 29.91531716123279239, -1.660698994484458346 ) ) ;
#3685 = VERTEX_POINT ( 'NONE', #5285 ) ;
#3686 = CARTESIAN_POINT ( 'NONE',  ( -1.854454310345000190, 24.53117208695000073, -1.420007133126999888 ) ) ;
#3687 = CARTESIAN_POINT ( 'NONE',  ( 20.61135635202220939, 6.753515711663456322, 8.075049422923598286 ) ) ;
#3688 = CARTESIAN_POINT ( 'NONE',  ( -0.9472309125058132606, 23.62634780752645014, -1.903746509698968081 ) ) ;
#3689 = EDGE_LOOP ( 'NONE', ( #14860, #16787, #12860, #8889, #5454, #12201 ) ) ;
#3690 = CARTESIAN_POINT ( 'NONE',  ( 24.28455689590299826, -3.990707743057282819, 12.50000000000000355 ) ) ;
#3691 = CARTESIAN_POINT ( 'NONE',  ( 5.065664929567285313, 14.06852716411717630, -3.939930271556426167 ) ) ;
#3692 = CARTESIAN_POINT ( 'NONE',  ( 4.776902136988002923, 12.47834512453000144, 0.1510561884015998724 ) ) ;
#3693 = CARTESIAN_POINT ( 'NONE',  ( 11.50200125730999900, -7.192471199227000511, -5.535041905695000430 ) ) ;
#3694 = ORIENTED_EDGE ( 'NONE', *, *, #18513, .F. ) ;
#3695 = VECTOR ( 'NONE', #7844, 1000.000000000000000 ) ;
#3696 = DIRECTION ( 'NONE',  ( 0.000000000000000000, 0.000000000000000000, 1.000000000000000000 ) ) ;
#3697 = SHAPE_DEFINITION_REPRESENTATION ( #11928, #16160 ) ;
#3698 = CARTESIAN_POINT ( 'NONE',  ( -14.33281117768507507, 5.151946275820663779, -12.49999999999962874 ) ) ;
#3699 = ORIENTED_EDGE ( 'NONE', *, *, #8801, .F. ) ;
#3700 = CARTESIAN_POINT ( 'NONE',  ( -15.91276253787999728, 9.079634562165001199, 0.000000000000000000 ) ) ;
#3701 = CARTESIAN_POINT ( 'NONE',  ( -24.22413361922000163, -2.219501623213000485, 9.414378356634001577 ) ) ;
#3702 = CARTESIAN_POINT ( 'NONE',  ( -15.15190331421999836, -2.304711170240999696, 9.446210836873998318 ) ) ;
#3703 = DIRECTION ( 'NONE',  ( 0.000000000000000000, 1.000000000000000000, 0.000000000000000000 ) ) ;
#3704 = CARTESIAN_POINT ( 'NONE',  ( -22.59459620538663316, 1.415938697088058307, -10.58759565406335135 ) ) ;
#3705 = CARTESIAN_POINT ( 'NONE',  ( -4.000000000000000000, 26.20000000000000284, -2.309401076759000304 ) ) ;
#3706 = DIRECTION ( 'NONE',  ( -0.5000000000000169864, 0.000000000000000000, -0.8660254037844288266 ) ) ;
#3707 = PLANE ( 'NONE',  #14292 ) ;
#3708 = EDGE_CURVE ( 'NONE', #3316, #12335, #152, .T. ) ;
#3709 = AXIS2_PLACEMENT_3D ( 'NONE', #21622, #3100, #17989 ) ;
#3710 = CARTESIAN_POINT ( 'NONE',  ( 2.013323156743944686, 30.65106894508059199, -0.7821756420678627197 ) ) ;
#3711 = ORIENTED_EDGE ( 'NONE', *, *, #4507, .F. ) ;
#3712 = B_SPLINE_CURVE_WITH_KNOTS ( 'NONE', 3,
 ( #13139, #3939, #16649, #7094, #55, #14484, #5286, #3480, #3820, #7440, #14820, #1648, #9038, #9386, #7559, #14937, #8927, #23799 ),
 .UNSPECIFIED., .F., .F.,
 ( 4, 2, 2, 2, 2, 2, 2, 2, 4 ),
 ( 0.000000000000000000, 0.1250000000000000000, 0.2500000000000000000, 0.3750000000000000000, 0.5000000000000000000, 0.6250000000000000000, 0.7500000000000000000, 0.8750000000000000000, 1.000000000000000000 ),
 .UNSPECIFIED. ) ;
#3713 = LINE ( 'NONE', #19841, #10401 ) ;
#3714 = CARTESIAN_POINT ( 'NONE',  ( 4.436745834877500627, 13.45903375662160073, -5.214346380604272468 ) ) ;
#3715 = AXIS2_PLACEMENT_3D ( 'NONE', #11917, #23037, #19302 ) ;
#3716 = CARTESIAN_POINT ( 'NONE',  ( -21.82243491649035505, 9.089534782749435493, 5.598433407583303989 ) ) ;
#3717 = CARTESIAN_POINT ( 'NONE',  ( -1.360883606431000148, 26.33937716036000154, 2.036706090186000129 ) ) ;
#3718 = FACE_OUTER_BOUND ( 'NONE', #738, .T. ) ;
#3719 = DIRECTION ( 'NONE',  ( 0.000000000000000000, -1.000000000000000000, 0.000000000000000000 ) ) ;
#3720 = ORIENTED_EDGE ( 'NONE', *, *, #21985, .F. ) ;
#3721 = CARTESIAN_POINT ( 'NONE',  ( -4.658304025590487285, 12.37774214680684892, -1.339611838526547416 ) ) ;
#3722 = EDGE_CURVE ( 'NONE', #5602, #23163, #22594, .T. ) ;
#3723 = CARTESIAN_POINT ( 'NONE',  ( -24.12232999016000079, 1.520060141252000183E-14, 0.000000000000000000 ) ) ;
#3724 = CARTESIAN_POINT ( 'NONE',  ( -0.8447332559524692863, 29.87863817527814803, -2.115577172688746455 ) ) ;
#3725 = ORIENTED_EDGE ( 'NONE', *, *, #9118, .T. ) ;
#3726 = CARTESIAN_POINT ( 'NONE',  ( 23.99062354302999722, -7.716878364870000340, 11.63397459621999985 ) ) ;
#3727 = AXIS2_PLACEMENT_3D ( 'NONE', #22979, #2522, #15350 ) ;
#3728 = CONICAL_SURFACE ( 'NONE', #4905, 4.649999926447000220, 0.7853981633972997312 ) ;
#3729 = CARTESIAN_POINT ( 'NONE',  ( 14.18737658531000001, 3.962519675866999602, -9.360324180111000203 ) ) ;
#3730 = CARTESIAN_POINT ( 'NONE',  ( 18.25830969247345337, 5.725820681186363004, -8.709654033915940730 ) ) ;
#3731 = CARTESIAN_POINT ( 'NONE',  ( 0.6543697108982093891, 29.26753006952333536, 2.434931691670787490 ) ) ;
#3732 = CARTESIAN_POINT ( 'NONE',  ( 2.140718310772999899, 30.55600469983999901, -0.2075533484111000138 ) ) ;
#3733 = DIRECTION ( 'NONE',  ( 0.000000000000000000, -1.000000000000000000, 0.000000000000000000 ) ) ;
#3734 = FACE_OUTER_BOUND ( 'NONE', #23498, .T. ) ;
#3735 = EDGE_LOOP ( 'NONE', ( #18257, #3233 ) ) ;
#3736 = CARTESIAN_POINT ( 'NONE',  ( 0.000000000000000000, 9.000000000000000000, 0.000000000000000000 ) ) ;
#3737 = CARTESIAN_POINT ( 'NONE',  ( 24.64508424622000149, 0.3734825580707000214, 10.84342182217999984 ) ) ;
#3738 = EDGE_CURVE ( 'NONE', #21095, #4782, #17080, .T. ) ;
#3739 = CARTESIAN_POINT ( 'NONE',  ( 0.6543697108982240440, 29.03333333333333854, 2.434931691670783049 ) ) ;
#3740 = VERTEX_POINT ( 'NONE', #7438 ) ;
#3741 = DIRECTION ( 'NONE',  ( 0.000000000000000000, 0.9899013191676121481, -0.1417581684074016302 ) ) ;
#3742 = CARTESIAN_POINT ( 'NONE',  ( -23.74465998031000069, 6.216878364870000340, -12.50000000000000000 ) ) ;
#3743 = CARTESIAN_POINT ( 'NONE',  ( 1.673168206979000594, 11.57251234639000970, 4.644218459094000551 ) ) ;
#3744 = AXIS2_PLACEMENT_3D ( 'NONE', #15710, #9917, #2780 ) ;
#3745 = CARTESIAN_POINT ( 'NONE',  ( 0.01500812129314476814, 29.20288496623757979, -2.161759760356441795 ) ) ;
#3746 = CARTESIAN_POINT ( 'NONE',  ( 0.000000000000000000, 9.050044887908999414, 0.000000000000000000 ) ) ;
#3747 = ORIENTED_EDGE ( 'NONE', *, *, #6285, .F. ) ;
#3748 = AXIS2_PLACEMENT_3D ( 'NONE', #15505, #2436, #4498 ) ;
#3749 = DIRECTION ( 'NONE',  ( 0.000000000000000000, 6.254606381427999609E-11, 1.000000000000000000 ) ) ;
#3750 = ORIENTED_EDGE ( 'NONE', *, *, #17334, .T. ) ;
#3751 = CARTESIAN_POINT ( 'NONE',  ( 1.941085051938999939, 25.12563408233999951, -1.330354224329999946 ) ) ;
#3752 = CARTESIAN_POINT ( 'NONE',  ( 4.972623340256002500, 14.42132507220000015, 3.509556516286003625 ) ) ;
#3753 = ADVANCED_FACE ( 'NONE', ( #21991 ), #14819, .T. ) ;
#3754 = CARTESIAN_POINT ( 'NONE',  ( 5.752357458139003121, 13.85427084562999589, 4.060679559109004799 ) ) ;
#3755 = CARTESIAN_POINT ( 'NONE',  ( -16.85755420454665554, -9.103879778418416890, 1.191568128638077262 ) ) ;
#3756 = DIRECTION ( 'NONE',  ( 0.000000000000000000, 0.7071067811866525998, -0.7071067811864425456 ) ) ;
#3757 = CARTESIAN_POINT ( 'NONE',  ( 11.88393908531000065, -9.721606288483000569, -2.753149205743999683 ) ) ;
#3758 = DIRECTION ( 'NONE',  ( 1.000000000000000000, 0.000000000000000000, 0.000000000000000000 ) ) ;
#3759 = ORIENTED_EDGE ( 'NONE', *, *, #13773, .F. ) ;
#3760 = CARTESIAN_POINT ( 'NONE',  ( -12.91415807507000046, -6.873022849445000304, -6.789234046460999927 ) ) ;
#3761 = AXIS2_PLACEMENT_3D ( 'NONE', #4996, #975, #15504 ) ;
#3762 = DIRECTION ( 'NONE',  ( 0.000000000000000000, 1.000000000000000000, 0.000000000000000000 ) ) ;
#3763 = EDGE_CURVE ( 'NONE', #11168, #20706, #20819, .T. ) ;
#3764 = CARTESIAN_POINT ( 'NONE',  ( -10.04281598263999875, 1.347635823622999967E-14, 0.000000000000000000 ) ) ;
#3765 = ORIENTED_EDGE ( 'NONE', *, *, #16914, .T. ) ;
#3766 = CARTESIAN_POINT ( 'NONE',  ( -10.71135110314821404, 15.41046848462710983, -1.565338808390349445 ) ) ;
#3767 = AXIS2_PLACEMENT_3D ( 'NONE', #3969, #9535, #16912 ) ;
#3768 = CARTESIAN_POINT ( 'NONE',  ( -1.814669259075999852, 24.47173345458000071, 1.469565487754999955 ) ) ;
#3769 = CARTESIAN_POINT ( 'NONE',  ( 14.65012636277685587, 6.238725812500826251, -8.226221173691849131 ) ) ;
#3770 = CARTESIAN_POINT ( 'NONE',  ( -5.194121241700999647, -12.44999999995000017, -4.899859737990999515E-10 ) ) ;
#3771 = CARTESIAN_POINT ( 'NONE',  ( 19.09627401310000039, -4.616208307064000316, 10.16717727690999951 ) ) ;
#3772 = EDGE_CURVE ( 'NONE', #7943, #18240, #18595, .T. ) ;
#3773 = CARTESIAN_POINT ( 'NONE',  ( 2.512136363505000247, 30.30246990879999913, -0.4555555407424999870 ) ) ;
#3774 = CARTESIAN_POINT ( 'NONE',  ( 13.80174867965053664, 9.025293717818129835, 0.002229559405347460773 ) ) ;
#3775 = EDGE_CURVE ( 'NONE', #8097, #20600, #9153, .T. ) ;
#3776 = CARTESIAN_POINT ( 'NONE',  ( -6.442648543447514697, 15.51394528351816327, -1.396635598960656921 ) ) ;
#3777 = CARTESIAN_POINT ( 'NONE',  ( -14.00000000000000000, -10.59999999999999964, 0.000000000000000000 ) ) ;
#3778 = CARTESIAN_POINT ( 'NONE',  ( 21.29840273415999619, -9.313682482016000463, -6.615575153290000010 ) ) ;
#3779 = ORIENTED_EDGE ( 'NONE', *, *, #16205, .F. ) ;
#3780 = DIRECTION ( 'NONE',  ( -2.317847129507103042E-07, 0.9999999999999731326, 0.000000000000000000 ) ) ;
#3781 = CIRCLE ( 'NONE', #18111, 7.500000000000000000 ) ;
#3782 = ORIENTED_EDGE ( 'NONE', *, *, #16185, .T. ) ;
#3783 = CARTESIAN_POINT ( 'NONE',  ( -15.69191243917330780, 8.837844618163940069, -2.374974410327074903 ) ) ;
#3784 = DIRECTION ( 'NONE',  ( 0.000000000000000000, 0.000000000000000000, 1.000000000000000000 ) ) ;
#3785 = ADVANCED_FACE ( 'NONE', ( #15536 ), #11802, .T. ) ;
#3786 = CARTESIAN_POINT ( 'NONE',  ( 22.21149770046333671, -9.241272520592698214, 1.209806691843540838 ) ) ;
#3787 = ADVANCED_FACE ( 'NONE', ( #22923 ), #21000, .F. ) ;
#3788 = CARTESIAN_POINT ( 'NONE',  ( 13.93747899715999949, -10.35476673622000021, -3.712727401404000371 ) ) ;
#3789 = FACE_OUTER_BOUND ( 'NONE', #18293, .T. ) ;
#3790 = CARTESIAN_POINT ( 'NONE',  ( -2.607696352436000176, 25.90712896666999754, 0.5721489135198000175 ) ) ;
#3791 = VERTEX_POINT ( 'NONE', #11447 ) ;
#3792 = CARTESIAN_POINT ( 'NONE',  ( -9.113751972103999677, 13.51820841023999975, -6.295940148715000184 ) ) ;
#3793 = CYLINDRICAL_SURFACE ( 'NONE', #23685, 1.000000000000000000 ) ;
#3794 = CARTESIAN_POINT ( 'NONE',  ( -14.47793701804645927, -11.73188619686388812, -4.679765522767608488 ) ) ;
#3795 = ORIENTED_EDGE ( 'NONE', *, *, #16810, .F. ) ;
#3796 = CARTESIAN_POINT ( 'NONE',  ( 1.699999999999999956, 9.029776626192267841, 0.9151613154069033751 ) ) ;
#3797 = CARTESIAN_POINT ( 'NONE',  ( 20.69983103379664868, -5.655443772474994191, -7.358828497896286791 ) ) ;
#3798 = CARTESIAN_POINT ( 'NONE',  ( 6.241905009026717188, 13.66125922203571363, 1.775230544922867582 ) ) ;
#3799 = CARTESIAN_POINT ( 'NONE',  ( 15.90676250867264052, -9.944674072179898516, -2.897521108056326344 ) ) ;
#3800 = AXIS2_PLACEMENT_3D ( 'NONE', #16933, #6028, #11264 ) ;
#3801 = CARTESIAN_POINT ( 'NONE',  ( -13.93024972067999911, -7.625744536618999092, 7.913094424807001204 ) ) ;
#3802 = CARTESIAN_POINT ( 'NONE',  ( -0.3395901671559999890, 28.81242903415000001, 2.083925050886000108 ) ) ;
#3803 = CARTESIAN_POINT ( 'NONE',  ( -17.22065346366999705, -7.714380452752999773, 6.849660182178999968 ) ) ;
#3804 = AXIS2_PLACEMENT_3D ( 'NONE', #590, #19509, #15608 ) ;
#3805 = CARTESIAN_POINT ( 'NONE',  ( -0.07097743868425297753, 29.59969681156075438, 2.158689068696717950 ) ) ;
#3806 = ORIENTED_EDGE ( 'NONE', *, *, #4172, .T. ) ;
#3807 = CARTESIAN_POINT ( 'NONE',  ( 0.5132826282582999555, 24.04258772846000269, 2.278587698102000125 ) ) ;
#3808 = CARTESIAN_POINT ( 'NONE',  ( 20.78159665399543243, 1.123289875192744480, 10.47162823820594468 ) ) ;
#3809 = CARTESIAN_POINT ( 'NONE',  ( -0.8709342061498644982, 23.65006605176747456, -1.965773624965944100 ) ) ;
#3810 = CIRCLE ( 'NONE', #22754, 0.8000000000000003775 ) ;
#3811 = ORIENTED_EDGE ( 'NONE', *, *, #17878, .F. ) ;
#3812 = CARTESIAN_POINT ( 'NONE',  ( -4.000000000000000000, 28.00000000000000000, -2.309401076759000304 ) ) ;
#3813 = ADVANCED_FACE ( 'NONE', ( #22455 ), #1324, .F. ) ;
#3814 = ADVANCED_FACE ( 'NONE', ( #22572 ), #641, .T. ) ;
#3815 = AXIS2_PLACEMENT_3D ( 'NONE', #17667, #15474, #1064 ) ;
#3816 = FACE_OUTER_BOUND ( 'NONE', #7547, .T. ) ;
#3817 = CARTESIAN_POINT ( 'NONE',  ( 17.45156392131000089, -0.08049851871593999286, -9.740865876825999692 ) ) ;
#3818 = EDGE_LOOP ( 'NONE', ( #17214, #17518, #7752, #6892 ) ) ;
#3819 = CARTESIAN_POINT ( 'NONE',  ( -4.142610502493168312, 15.10207515396060352, 4.511673133457231089 ) ) ;
#3820 = CARTESIAN_POINT ( 'NONE',  ( -0.3272492347489287523, 29.78333333333333499, 2.500000000000001332 ) ) ;
#3821 = AXIS2_PLACEMENT_3D ( 'NONE', #8561, #21392, #21147 ) ;
#3822 = ORIENTED_EDGE ( 'NONE', *, *, #4195, .F. ) ;
#3823 = CARTESIAN_POINT ( 'NONE',  ( 22.51383103379667361, -5.684051423272225456, -7.396053641303423909 ) ) ;
#3824 = CARTESIAN_POINT ( 'NONE',  ( 4.738540299664001587, 12.61405493002000711, 0.2471290196958000063 ) ) ;
#3825 = AXIS2_PLACEMENT_3D ( 'NONE', #9780, #18980, #2391 ) ;
#3826 = CARTESIAN_POINT ( 'NONE',  ( -20.53063986495000037, -4.235883636776000216, 8.584601015509999655 ) ) ;
#3827 = CARTESIAN_POINT ( 'NONE',  ( 19.03699770046332418, -1.199143088786338796, -9.159808593981743741 ) ) ;
#3828 = DIRECTION ( 'NONE',  ( 0.000000000000000000, -1.000000000000000000, 0.000000000000000000 ) ) ;
#3829 = LINE ( 'NONE', #13469, #6944 ) ;
#3830 = CARTESIAN_POINT ( 'NONE',  ( -24.50000000000000000, 1.524685264937999788E-14, 0.000000000000000000 ) ) ;
#3831 = VECTOR ( 'NONE', #20193, 1000.000000000000000 ) ;
#3832 = CARTESIAN_POINT ( 'NONE',  ( 15.61599999999999966, 9.072019050554999353, 0.000000000000000000 ) ) ;
#3833 = CARTESIAN_POINT ( 'NONE',  ( 18.51344355829000321, 6.966878364870000340, 12.06698729810999993 ) ) ;
#3834 = CARTESIAN_POINT ( 'NONE',  ( 1.456462752601113353, 30.70952715242214381, -1.595930482832717434 ) ) ;
#3835 = EDGE_LOOP ( 'NONE', ( #1409, #16851, #12026, #2074, #23143 ) ) ;
#3836 = CARTESIAN_POINT ( 'NONE',  ( 6.696152422707000618, 29.50000000000000000, 115.0195023120000002 ) ) ;
#3837 = CARTESIAN_POINT ( 'NONE',  ( 14.09123181476553910, 9.084527387259015541, 0.1472698650368901852 ) ) ;
#3838 = CIRCLE ( 'NONE', #9642, 2.270871215252209030 ) ;
#3839 = CARTESIAN_POINT ( 'NONE',  ( -23.16125366752128656, -6.188651670778435587, 8.573940610315684552 ) ) ;
#3840 = CARTESIAN_POINT ( 'NONE',  ( 0.4021892318948999678, 26.45521896306000187, 2.252185756629999869 ) ) ;
#3841 = DIRECTION ( 'NONE',  ( 0.000000000000000000, -1.000000000000000000, 0.000000000000000000 ) ) ;
#3842 = CIRCLE ( 'NONE', #8504, 15.45000000000000107 ) ;
#3843 = CARTESIAN_POINT ( 'NONE',  ( 4.690616603563839249, 12.38867937097142757, 1.313715200103743763 ) ) ;
#3844 = ORIENTED_EDGE ( 'NONE', *, *, #20912, .F. ) ;
#3845 = CARTESIAN_POINT ( 'NONE',  ( -1.948370167467705638, 11.64426098586311831, -4.406099265893608674 ) ) ;
#3846 = CARTESIAN_POINT ( 'NONE',  ( 24.37173283531059909, 12.35285683711744653, 3.604224339486718609 ) ) ;
#3847 = CIRCLE ( 'NONE', #16228, 2.100000000000000089 ) ;
#3848 = CARTESIAN_POINT ( 'NONE',  ( 4.834857269758976450, 12.45115135844470622, 0.1243267821587187988 ) ) ;
#3849 = EDGE_LOOP ( 'NONE', ( #9322, #10380, #8162 ) ) ;
#3850 = EDGE_CURVE ( 'NONE', #5360, #14220, #13360, .T. ) ;
#3851 = PLANE ( 'NONE',  #14600 ) ;
#3852 = CARTESIAN_POINT ( 'NONE',  ( 16.27143908530999639, 9.938600131338999333, -2.378686727414999869 ) ) ;
#3853 = CARTESIAN_POINT ( 'NONE',  ( 18.39512765608887435, 9.038824569696712885, -5.186684426708589868 ) ) ;
#3854 = VECTOR ( 'NONE', #3784, 1000.000000000000000 ) ;
#3855 = LINE ( 'NONE', #5439, #11567 ) ;
#3856 = CARTESIAN_POINT ( 'NONE',  ( -2.121370068014000410, 29.36476973129000001, 0.3543124420124999507 ) ) ;
#3857 = CARTESIAN_POINT ( 'NONE',  ( 14.71864037305999950, 1.512073574203999904, -10.68419109087999885 ) ) ;
#3858 = PLANE ( 'NONE',  #21283 ) ;
#3859 = AXIS2_PLACEMENT_3D ( 'NONE', #14426, #14540, #22274 ) ;
#3860 = ORIENTED_EDGE ( 'NONE', *, *, #13378, .F. ) ;
#3861 = DIRECTION ( 'NONE',  ( 0.000000000000000000, 0.000000000000000000, 1.000000000000000000 ) ) ;
#3862 = CARTESIAN_POINT ( 'NONE',  ( 24.76311698098999869, -3.832248145790000393, 9.673750008746999640 ) ) ;
#3863 = B_SPLINE_CURVE_WITH_KNOTS ( 'NONE', 3,
 ( #6865, #4573, #14257, #17531, #21655, #11965, #5068, #925 ),
 .UNSPECIFIED., .F., .F.,
 ( 4, 2, 2, 4 ),
 ( 0.000000000000000000, 0.2500000000000000000, 0.5000000000000000000, 1.000000000000000000 ),
 .UNSPECIFIED. ) ;
#3864 = CARTESIAN_POINT ( 'NONE',  ( -24.10634617653294498, 6.505742320928646016, 7.512631181061424357 ) ) ;
#3865 = ORIENTED_EDGE ( 'NONE', *, *, #18114, .T. ) ;
#3866 = CARTESIAN_POINT ( 'NONE',  ( -12.49585571294465325, 6.729692068040215247, -5.965106315427219918 ) ) ;
#3867 = CARTESIAN_POINT ( 'NONE',  ( 3.000000000000000000, 15.00000000000000000, 0.000000000000000000 ) ) ;
#3868 = CARTESIAN_POINT ( 'NONE',  ( 3.358145790808003905, 11.92291747373999478, 3.495386131071001934 ) ) ;
#3869 = CARTESIAN_POINT ( 'NONE',  ( -0.6469316270125009538, 29.24251007170759920, -2.063874927344320209 ) ) ;
#3870 = CARTESIAN_POINT ( 'NONE',  ( 12.52688711657000020, 13.93375672974000068, -0.8660254037843999608 ) ) ;
#3871 = ORIENTED_EDGE ( 'NONE', *, *, #22837, .T. ) ;
#3872 = CARTESIAN_POINT ( 'NONE',  ( -0.01212694170664108638, 23.76765559877391354, 2.284373250672524058 ) ) ;
#3873 = EDGE_LOOP ( 'NONE', ( #3237, #4591, #23086, #17175 ) ) ;
#3874 = CARTESIAN_POINT ( 'NONE',  ( 2.064511051236999961, 25.76334910003999923, -0.3253761041896999773 ) ) ;
#3875 = CARTESIAN_POINT ( 'NONE',  ( -7.500000000000000000, 24.99999999999999645, 1.000000000000000000 ) ) ;
#3876 = CARTESIAN_POINT ( 'NONE',  ( -2.256099604565999783, 27.67799822781000074, -0.2222064166828000287 ) ) ;
#3877 = CARTESIAN_POINT ( 'NONE',  ( 16.61833103379667165, -7.275071925230092162, 5.591076558181078404 ) ) ;
#3878 = DIRECTION ( 'NONE',  ( 0.000000000000000000, -1.000000000000000000, 0.000000000000000000 ) ) ;
#3879 = CARTESIAN_POINT ( 'NONE',  ( -12.25000000000000000, 1.374666032043000015E-14, 0.000000000000000000 ) ) ;
#3880 = DIRECTION ( 'NONE',  ( 0.000000000000000000, -1.000000000000000000, 0.000000000000000000 ) ) ;
#3881 = EDGE_CURVE ( 'NONE', #9228, #23352, #14481, .T. ) ;
#3882 = SHAPE_REPRESENTATION_RELATIONSHIP ( 'NONE' , 'NONE' ,  #16160, #982 ) ;
#3883 = CARTESIAN_POINT ( 'NONE',  ( -18.98111647941000157, -8.384220026111998791, 5.081857170174999716 ) ) ;
#3884 = B_SPLINE_CURVE_WITH_KNOTS ( 'NONE', 3,
 ( #2986, #6612, #19337, #4687, #12073, #19456, #4926, #14118, #909, #19702, #12312, #6848, #14241, #2864, #3117, #15676, #8191, #17639, #6363, #10501, #21513, #8437 ),
 .UNSPECIFIED., .F., .F.,
 ( 4, 2, 2, 1, 1, 2, 2, 2, 2, 2, 2, 4 ),
 ( 0.000000000000000000, 0.1250000000000900391, 0.1875000000001351697, 0.2187500000001618428, 0.2343750000001749989, 0.2421875000001745271, 0.2500000000001740830, 0.3750000000001458278, 0.4375000000001291744, 0.4687500000001231792, 0.5000000000001172396, 1.000000000000000000 ),
 .UNSPECIFIED. ) ;
#3885 = DIRECTION ( 'NONE',  ( 0.000000000000000000, -1.000000000000000000, 0.000000000000000000 ) ) ;
#3886 = DIRECTION ( 'NONE',  ( -0.000000000000000000, -1.000000000000000000, -0.000000000000000000 ) ) ;
#3887 = ORIENTED_EDGE ( 'NONE', *, *, #11874, .F. ) ;
#3888 = CARTESIAN_POINT ( 'NONE',  ( -21.36254453733999981, -7.691211596171000586, 8.186677943368000143 ) ) ;
#3889 = CARTESIAN_POINT ( 'NONE',  ( 2.229792775116000048, 24.02344565378000141, -0.6933047407275000351 ) ) ;
#3890 = CARTESIAN_POINT ( 'NONE',  ( 4.495027222853295257, 14.65432717051509037, -4.161727442053731352 ) ) ;
#3891 = DIRECTION ( 'NONE',  ( 0.000000000000000000, -1.000000000000000000, 0.000000000000000000 ) ) ;
#3892 = CARTESIAN_POINT ( 'NONE',  ( 21.29883756869999800, -11.00028630601000046, -2.245331027877000007 ) ) ;
#3893 = CARTESIAN_POINT ( 'NONE',  ( 0.6648189132885999886, 30.44608768000000154, -2.465032527426999742 ) ) ;
#3894 = EDGE_CURVE ( 'NONE', #12304, #20918, #14472, .T. ) ;
#3895 = CARTESIAN_POINT ( 'NONE',  ( 13.80113244728332234, 9.025301755077943966, -0.01720271198835989293 ) ) ;
#3896 = PLANE ( 'NONE',  #6122 ) ;
#3897 = CARTESIAN_POINT ( 'NONE',  ( 12.40357033522255037, 13.79529643152775797, -1.105845675118900084 ) ) ;
#3898 = VERTEX_POINT ( 'NONE', #4533 ) ;
#3899 = CARTESIAN_POINT ( 'NONE',  ( 1.800000000000000044, 13.00000000000000000, -1.081665382638999917 ) ) ;
#3900 = EDGE_CURVE ( 'NONE', #22764, #1513, #8294, .T. ) ;
#3901 = VERTEX_POINT ( 'NONE', #10103 ) ;
#3902 = CARTESIAN_POINT ( 'NONE',  ( 1.709999999999999964, 9.000000000000000000, -0.3720215047547999476 ) ) ;
#3903 = DIRECTION ( 'NONE',  ( -1.000000000000000000, 0.000000000000000000, 0.000000000000000000 ) ) ;
#3904 = DIRECTION ( 'NONE',  ( -1.000000000000000000, 0.000000000000000000, 0.000000000000000000 ) ) ;
#3905 = CARTESIAN_POINT ( 'NONE',  ( 18.41492214233000269, 10.39830466543000043, -3.948887927675999165 ) ) ;
#3906 = AXIS2_PLACEMENT_3D ( 'NONE', #1350, #15865, #8977 ) ;
#3907 = DIRECTION ( 'NONE',  ( -1.000000000000000000, 0.000000000000000000, 2.810008490046999894E-14 ) ) ;
#3908 = EDGE_CURVE ( 'NONE', #2909, #11168, #22263, .T. ) ;
#3909 = CARTESIAN_POINT ( 'NONE',  ( 2.159851832628000068, 26.19962896667000152, 1.569224139466999901 ) ) ;
#3910 = ORIENTED_EDGE ( 'NONE', *, *, #4655, .T. ) ;
#3911 = ORIENTED_EDGE ( 'NONE', *, *, #436, .T. ) ;
#3912 = B_SPLINE_CURVE_WITH_KNOTS ( 'NONE', 3,
 ( #3067, #19651, #16358, #10452, #23514, #19776, #18305, #5005, #16245, #1708, #5120, #14541, #18073, #5346, #17839, #1234, #3303, #5235, #9097, #12502, #12619, #8624, #10809, #18201 ),
 .UNSPECIFIED., .F., .F.,
 ( 4, 2, 2, 2, 2, 2, 2, 2, 2, 2, 2, 4 ),
 ( 8.179270553615951679E-05, 0.0008436736815539817337, 0.001224614169562892978, 0.001605554657571804439, 0.002367435633589626710, 0.002748376121598538387, 0.002938846365602994226, 0.003034081487605222362, 0.003057890268105779071, 0.003069794658356057859, 0.003081699048606336214, 0.003129316609607453534 ),
 .UNSPECIFIED. ) ;
#3913 = CARTESIAN_POINT ( 'NONE',  ( -10.81816756584999872, -7.700301352277000078, -12.71861605121999972 ) ) ;
#3914 = CARTESIAN_POINT ( 'NONE',  ( 0.000000000000000000, 18.50000000000000000, 0.000000000000000000 ) ) ;
#3915 = CARTESIAN_POINT ( 'NONE',  ( -14.45529025083969898, -9.532921455384554932, -8.488438081456083140 ) ) ;
#3916 = ORIENTED_EDGE ( 'NONE', *, *, #4864, .F. ) ;
#3917 = CARTESIAN_POINT ( 'NONE',  ( 20.11758333333333226, -9.187538551043507695, 1.063519409932076609 ) ) ;
#3918 = CARTESIAN_POINT ( 'NONE',  ( 19.58787013427168233, -4.214981502252697076, -9.617786801466230884 ) ) ;
#3919 = PLANE ( 'NONE',  #17237 ) ;
#3920 = CARTESIAN_POINT ( 'NONE',  ( 16.03245491809901324, -7.736135533815227561, -6.891731924576589563 ) ) ;
#3921 = CARTESIAN_POINT ( 'NONE',  ( -19.49677076852000113, -7.796036496380999381, 6.940746985983999195 ) ) ;
#3922 = CARTESIAN_POINT ( 'NONE',  ( -2.042928671780000371, 30.08837290161000055, 1.173968745881999842 ) ) ;
#3923 = EDGE_CURVE ( 'NONE', #9876, #15019, #3277, .T. ) ;
#3924 = CARTESIAN_POINT ( 'NONE',  ( -17.66767224083000087, -1.527991571549000005, 10.75645198264999891 ) ) ;
#3925 = CARTESIAN_POINT ( 'NONE',  ( 1.139808571972009021, 29.67456316804590699, 1.835980945443606238 ) ) ;
#3926 = ORIENTED_EDGE ( 'NONE', *, *, #2587, .T. ) ;
#3927 = CARTESIAN_POINT ( 'NONE',  ( -0.06876214361208000947, 24.82870495165000335, 2.180404198171999930 ) ) ;
#3928 = LINE ( 'NONE', #11321, #4627 ) ;
#3929 = CARTESIAN_POINT ( 'NONE',  ( -18.91964744305752077, 3.100836465720866020, -10.17440793236460728 ) ) ;
#3930 = VERTEX_POINT ( 'NONE', #15781 ) ;
#3931 = FACE_OUTER_BOUND ( 'NONE', #6802, .T. ) ;
#3932 = DIRECTION ( 'NONE',  ( -1.000000000000000000, 0.000000000000000000, 0.000000000000000000 ) ) ;
#3933 = CARTESIAN_POINT ( 'NONE',  ( -13.99999999999999822, -9.930093542707636445, 2.724120365425963364 ) ) ;
#3934 = EDGE_CURVE ( 'NONE', #11746, #4287, #16404, .T. ) ;
#3935 = CARTESIAN_POINT ( 'NONE',  ( 14.68293875730999964, -5.746474821545000111, 7.132383943660999925 ) ) ;
#3936 = EDGE_CURVE ( 'NONE', #1186, #2766, #16780, .T. ) ;
#3937 = ORIENTED_EDGE ( 'NONE', *, *, #5491, .T. ) ;
#3938 = CARTESIAN_POINT ( 'NONE',  ( -1.536366799937273653, 28.35086340285666395, 1.999167105995461213 ) ) ;
#3939 = CARTESIAN_POINT ( 'NONE',  ( -2.499999999999999556, 29.61666666666666714, 0.3272492347489423525 ) ) ;
#3940 = CIRCLE ( 'NONE', #17477, 2.500000000000000000 ) ;
#3941 = EDGE_LOOP ( 'NONE', ( #9150, #19213, #9707, #22563, #521 ) ) ;
#3942 = B_SPLINE_CURVE_WITH_KNOTS ( 'NONE', 3,
 ( #7537, #2788, #10173, #11993, #16083, #15960, #23353, #955, #19378, #19624, #6771, #12237, #17560, #3274, #4605, #12115, #3158, #23482, #8353, #8480, #21191, #12474 ),
 .UNSPECIFIED., .F., .F.,
 ( 4, 2, 2, 2, 2, 2, 2, 2, 2, 2, 4 ),
 ( 0.000000000000000000, 0.07385965502458807785, 0.1477193100491761557, 0.1846491375614701946, 0.2215789650737642613, 0.2954386200983524224, 0.3692982751229405558, 0.4431579301475287447, 0.4800877576598228669, 0.5170175851721169336, 0.5908772401967050669 ),
 .UNSPECIFIED. ) ;
#3943 = CARTESIAN_POINT ( 'NONE',  ( 1.768240990936880142, 24.49990546444021078, -1.767061324597003713 ) ) ;
#3944 = CARTESIAN_POINT ( 'NONE',  ( -1.044905824211999734, 11.67616894756002033, 4.654497658188999409 ) ) ;
#3945 = CARTESIAN_POINT ( 'NONE',  ( 12.00000000000000000, 0.3610762368853280280, -9.315579937737750171 ) ) ;
#3946 = CARTESIAN_POINT ( 'NONE',  ( -14.44633174692086008, 9.404057468167051681, -8.711677720880402376 ) ) ;
#3948 = ADVANCED_FACE ( 'NONE', ( #8539 ), #23762, .T. ) ;
#3947 = CARTESIAN_POINT ( 'NONE',  ( -4.014472954888002043, 13.57154522720001744, -4.599265107325998692 ) ) ;
#3949 = ADVANCED_FACE ( 'NONE', ( #16137 ), #4037, .F. ) ;
#3950 = DIRECTION ( 'NONE',  ( 1.000000000000000000, 0.000000000000000000, 0.000000000000000000 ) ) ;
#3951 = VECTOR ( 'NONE', #17436, 999.9999999999998863 ) ;
#3952 = SURFACE_SIDE_STYLE ('',( #20541 ) ) ;
#3953 = PLANE ( 'NONE',  #6041 ) ;
#3954 = CARTESIAN_POINT ( 'NONE',  ( 0.8670279822662322333, 30.45653399219317592, 1.978445612786488672 ) ) ;
#3955 = ORIENTED_EDGE ( 'NONE', *, *, #4832, .F. ) ;
#3956 = DIRECTION ( 'NONE',  ( 1.000000000000000000, 0.000000000000000000, 0.000000000000000000 ) ) ;
#3957 = CARTESIAN_POINT ( 'NONE',  ( 1.493398715743419869, 24.78022351799236489, 1.505750370948753414 ) ) ;
#3958 = CARTESIAN_POINT ( 'NONE',  ( -23.51536743654689943, -5.893785232171476984, -7.219491138192441149 ) ) ;
#3959 = CARTESIAN_POINT ( 'NONE',  ( -23.75033391797219906, 10.46611617202711031, 1.634913018610795632 ) ) ;
#3960 = CARTESIAN_POINT ( 'NONE',  ( -1.273605814386999713, 26.11364211382000278, 1.906085653762000121 ) ) ;
#3961 = CARTESIAN_POINT ( 'NONE',  ( -2.127716147605950514, 30.86060364257915367, 0.2232574844277085691 ) ) ;
#3962 = AXIS2_PLACEMENT_3D ( 'NONE', #21933, #6799, #14193 ) ;
#3963 = DIRECTION ( 'NONE',  ( 0.000000000000000000, -1.000000000000000000, 0.000000000000000000 ) ) ;
#3964 = VERTEX_POINT ( 'NONE', #3331 ) ;
#3965 = CARTESIAN_POINT ( 'NONE',  ( -3.261050669804293811, 11.92957528164763126, -3.562551734304618911 ) ) ;
#3966 = CARTESIAN_POINT ( 'NONE',  ( -10.90000000000000036, -7.100000000000000533, 0.000000000000000000 ) ) ;
#3967 = CARTESIAN_POINT ( 'NONE',  ( -4.000000000000057732, 28.25094615492120909, 2.107036910272269470 ) ) ;
#3968 = ORIENTED_EDGE ( 'NONE', *, *, #10594, .T. ) ;
#3969 = CARTESIAN_POINT ( 'NONE',  ( 0.000000000000000000, 18.00000000000000000, 0.000000000000000000 ) ) ;
#3970 = CARTESIAN_POINT ( 'NONE',  ( 13.30987658531000051, -4.885510779899000511, 8.887104416848000454 ) ) ;
#3971 = CARTESIAN_POINT ( 'NONE',  ( -19.42261965736999940, -11.41835772389999981, 0.8203659406909000751 ) ) ;
#3972 = PLANE ( 'NONE',  #17357 ) ;
#3973 = CARTESIAN_POINT ( 'NONE',  ( 13.90614037306000128, -4.856636860576000636, 9.610582908496999366 ) ) ;
#3974 = CARTESIAN_POINT ( 'NONE',  ( 1.236794719700695211, 24.50000548481460427, 2.172625763342098004 ) ) ;
#3975 = AXIS2_PLACEMENT_3D ( 'NONE', #15262, #19146, #15385 ) ;
#3976 = FACE_OUTER_BOUND ( 'NONE', #19466, .T. ) ;
#3977 = CARTESIAN_POINT ( 'NONE',  ( 20.39590579450999996, 8.765676152204999738, -6.195664695497000274 ) ) ;
#3978 = DIRECTION ( 'NONE',  ( 0.000000000000000000, 1.000000000000000000, 0.000000000000000000 ) ) ;
#3979 = ORIENTED_EDGE ( 'NONE', *, *, #8769, .T. ) ;
#3980 = DIRECTION ( 'NONE',  ( 0.000000000000000000, 0.000000000000000000, 1.000000000000000000 ) ) ;
#3981 = CARTESIAN_POINT ( 'NONE',  ( 24.50000000000000000, -1.131740379468156865, 10.47946835040394298 ) ) ;
#3982 = CARTESIAN_POINT ( 'NONE',  ( 4.673640587513999023, 12.34837631718999340, 1.539931574126999880 ) ) ;
#3983 = CARTESIAN_POINT ( 'NONE',  ( -1.569329342329819577, 29.30733016622408371, -1.486957734784279062 ) ) ;
#3984 = CARTESIAN_POINT ( 'NONE',  ( -19.33846693354000124, -10.46074197849999976, 1.868315815290999993 ) ) ;
#3985 = VERTEX_POINT ( 'NONE', #12417 ) ;
#3986 = CARTESIAN_POINT ( 'NONE',  ( 12.00000000000000000, 0.000000000000000000, 0.000000000000000000 ) ) ;
#3987 = VERTEX_POINT ( 'NONE', #1010 ) ;
#3988 = CARTESIAN_POINT ( 'NONE',  ( -1.155917513699999954, 24.67184805413999982, 1.826172021010999957 ) ) ;
#3989 = CARTESIAN_POINT ( 'NONE',  ( 6.273729641689004488, 13.70226080931000467, -0.03746541131887003856 ) ) ;
#3990 = CARTESIAN_POINT ( 'NONE',  ( -0.2222064166829000043, 26.70299822781000287, -2.256099604565999783 ) ) ;
#3991 = FACE_OUTER_BOUND ( 'NONE', #21871, .T. ) ;
#3992 = CARTESIAN_POINT ( 'NONE',  ( 11.31235608929908665, 2.505169353248475783, -12.49996790082812659 ) ) ;
#3993 = CARTESIAN_POINT ( 'NONE',  ( 23.99478584076000232, -13.93375672974000068, 0.6736217021363000157 ) ) ;
#3994 = DIRECTION ( 'NONE',  ( 1.000000000000000000, 0.000000000000000000, 0.000000000000000000 ) ) ;
#3995 = CARTESIAN_POINT ( 'NONE',  ( -13.80819562941000100, -8.705043851576000691, 6.319240472362000816 ) ) ;
#3996 = CARTESIAN_POINT ( 'NONE',  ( 61.60588651278290939, 74.97299614839606363, 1.000000000000000000 ) ) ;
#3997 = CARTESIAN_POINT ( 'NONE',  ( -14.44097977831989255, -2.973612400777547737, 12.49999313495312414 ) ) ;
#3998 = VERTEX_POINT ( 'NONE', #6591 ) ;
#3999 = SURFACE_STYLE_USAGE ( .BOTH. , #18765 ) ;
#4000 = CARTESIAN_POINT ( 'NONE',  ( 1.751540416571000236, 23.98205213760000021, -1.819511229224000104 ) ) ;
#4001 = CARTESIAN_POINT ( 'NONE',  ( 14.19326017626335279, -8.265447570964310486, -6.165922807610080270 ) ) ;
#4002 = DIRECTION ( 'NONE',  ( -0.7071067811864758523, 0.7071067811861759811, -7.917084064338729087E-07 ) ) ;
#4003 = CARTESIAN_POINT ( 'NONE',  ( 19.31674634214999742, -11.08266600408999913, -1.414964896437999942 ) ) ;
#4004 = CARTESIAN_POINT ( 'NONE',  ( -2.360231394774000346, 29.18715348418999866, 0.03874416005483000136 ) ) ;
#4005 = CARTESIAN_POINT ( 'NONE',  ( 13.79403029713875561, 9.023035438857904822, -0.2363099913121846085 ) ) ;
#4006 = CARTESIAN_POINT ( 'NONE',  ( -6.838539683295000060, 15.31903503039000114, -1.878299264234999821 ) ) ;
#4007 = CARTESIAN_POINT ( 'NONE',  ( 0.000000000000000000, 9.000000000000000000, -1.899912543625706274 ) ) ;
#4008 = ADVANCED_FACE ( 'NONE', ( #1383 ), #8811, .F. ) ;
#4009 = CARTESIAN_POINT ( 'NONE',  ( 11.18574820343221710, 9.950120879851732880, -7.765924039707254423 ) ) ;
#4010 = EDGE_LOOP ( 'NONE', ( #13966, #3564, #428 ) ) ;
#4011 = CARTESIAN_POINT ( 'NONE',  ( -2.430432513736672906, 24.27082020183427247, 0.7153544994183682615 ) ) ;
#4012 = CYLINDRICAL_SURFACE ( 'NONE', #4190, 4.750000000000000000 ) ;
#4013 = ORIENTED_EDGE ( 'NONE', *, *, #22806, .F. ) ;
#4014 = CARTESIAN_POINT ( 'NONE',  ( 19.28343529110456700, -1.811640167859055017, 9.852238740839766251 ) ) ;
#4015 = CIRCLE ( 'NONE', #16389, 2.500000000000000000 ) ;
#4016 = DIRECTION ( 'NONE',  ( 0.000000000000000000, 1.000000000000000000, 0.000000000000000000 ) ) ;
#4017 = CARTESIAN_POINT ( 'NONE',  ( -1.595510613210902484, 29.99040384242091406, -3.697633671484739537 ) ) ;
#4018 = ORIENTED_EDGE ( 'NONE', *, *, #2556, .T. ) ;
#4019 = CARTESIAN_POINT ( 'NONE',  ( 13.21567540576999988, 5.680959247587999528, 8.577876493359001486 ) ) ;
#4020 = DIRECTION ( 'NONE',  ( -1.000000000000000000, 0.000000000000000000, 0.000000000000000000 ) ) ;
#4021 = CARTESIAN_POINT ( 'NONE',  ( -2.254705796085000102, 27.45919433610000127, 1.777466727206999941 ) ) ;
#4022 = EDGE_CURVE ( 'NONE', #14442, #18459, #4966, .T. ) ;
#4023 = VERTEX_POINT ( 'NONE', #22544 ) ;
#4024 = ORIENTED_EDGE ( 'NONE', *, *, #2604, .F. ) ;
#4025 = CARTESIAN_POINT ( 'NONE',  ( -14.00000000000000355, 3.517902211551271474, -8.602570206292373456 ) ) ;
#4026 = CARTESIAN_POINT ( 'NONE',  ( 1.536366799937286087, 27.15086340285666822, -1.999167105995451221 ) ) ;
#4027 = LINE ( 'NONE', #5724, #21372 ) ;
#4028 = CONICAL_SURFACE ( 'NONE', #4406, 2.949999959913000236, 0.7853981633972997312 ) ;
#4029 = CARTESIAN_POINT ( 'NONE',  ( -6.838539683295000060, 15.31903503039000114, -1.878299264234999821 ) ) ;
#4030 = ORIENTED_EDGE ( 'NONE', *, *, #18897, .F. ) ;
#4031 = CARTESIAN_POINT ( 'NONE',  ( -14.49454882815140522, 10.37180012737163359, 7.035449704349444389 ) ) ;
#4032 = CARTESIAN_POINT ( 'NONE',  ( 21.26670603379664470, 8.977084173768046682, -2.412654681333150197 ) ) ;
#4033 = CARTESIAN_POINT ( 'NONE',  ( 6.154060171291465764, 14.10599882039383779, 0.3200240209268620517 ) ) ;
#4034 = CARTESIAN_POINT ( 'NONE',  ( 15.75691745686210510, -10.07139243573377030, 2.399251823897887714 ) ) ;
#4035 = CARTESIAN_POINT ( 'NONE',  ( -16.06416778292000203, -1.832745140302000086, 10.89464230799999989 ) ) ;
#4036 = CARTESIAN_POINT ( 'NONE',  ( 0.4726444045413000228, 28.61631019869999903, 2.141105848461999805 ) ) ;
#4037 = TOROIDAL_SURFACE ( 'NONE', #2889, 2.099999992707999752, 0.1000000000000000056 ) ;
#4038 = CARTESIAN_POINT ( 'NONE',  ( -18.72408206190999991, 5.159378177076999528, -10.19862909758999869 ) ) ;
#4039 = EDGE_CURVE ( 'NONE', #18459, #2273, #17553, .T. ) ;
#4040 = CARTESIAN_POINT ( 'NONE',  ( 0.7411338969787365505, 29.64842732084730770, 2.029636956427176120 ) ) ;
#4041 = ORIENTED_EDGE ( 'NONE', *, *, #12836, .F. ) ;
#4042 = CARTESIAN_POINT ( 'NONE',  ( -0.07362252012096999476, 24.81036314894999961, 2.334523671301000469 ) ) ;
#4043 = CARTESIAN_POINT ( 'NONE',  ( -24.50000000000000355, -6.320988460424660893, -8.473731186276276972 ) ) ;
#4044 = AXIS2_PLACEMENT_3D ( 'NONE', #17253, #21262, #23052 ) ;
#4045 = CARTESIAN_POINT ( 'NONE',  ( 5.302309017544000191, 13.73032573480000096, -4.450985556070999216 ) ) ;
#4046 = EDGE_LOOP ( 'NONE', ( #20719, #17660 ) ) ;
#4047 = CARTESIAN_POINT ( 'NONE',  ( 2.424643331163519964E-11, 24.52694564545263844, -2.373054354547839306 ) ) ;
#4048 = CARTESIAN_POINT ( 'NONE',  ( 1.950358564618835500, 30.32279782412667402, -1.623347314877277459 ) ) ;
#4049 = CARTESIAN_POINT ( 'NONE',  ( -23.74228231688656976, 8.693394395448456762E-05, -9.522797051439189531 ) ) ;
#4050 = ADVANCED_FACE ( 'NONE', ( #21309 ), #4722, .T. ) ;
#4051 = CARTESIAN_POINT ( 'NONE',  ( 11.94075125730999964, 5.167059442038000050, -7.475232529384999047 ) ) ;
#4052 = VERTEX_POINT ( 'NONE', #10414 ) ;
#4053 = CARTESIAN_POINT ( 'NONE',  ( -5.989773396780996961, 16.41865079481998890, -1.007191989855000358 ) ) ;
#4054 = CARTESIAN_POINT ( 'NONE',  ( 24.45564077607145492, -11.85537957198067005, 4.465880238315118156 ) ) ;
#4055 = EDGE_LOOP ( 'NONE', ( #16683, #7350, #19085, #18273, #4428, #4436, #6358, #5880, #18247 ) ) ;
#4056 = CARTESIAN_POINT ( 'NONE',  ( -16.51742920454665509, -4.580373640694110016, -7.947268161980230339 ) ) ;
#4057 = CARTESIAN_POINT ( 'NONE',  ( 0.000000000000000000, 24.50000000000000000, -2.400000000000455991 ) ) ;
#4058 = CARTESIAN_POINT ( 'NONE',  ( 1.613427892151998666, 11.77489200500998834, 4.557952326475001925 ) ) ;
#4059 = AXIS2_PLACEMENT_3D ( 'NONE', #9220, #22061, #20484 ) ;
#4060 = ADVANCED_FACE ( 'NONE', ( #23823 ), #252, .T. ) ;
#4061 = CARTESIAN_POINT ( 'NONE',  ( -24.38472030418999736, 3.087124291345999971, 9.171168033639998995 ) ) ;
#4062 = CARTESIAN_POINT ( 'NONE',  ( 18.65908103379666372, -9.150110507480414768, -1.197619716921026090 ) ) ;
#4063 = CARTESIAN_POINT ( 'NONE',  ( -4.796844195024712043, 13.32315443175082414, 5.553764072526095497 ) ) ;
#4064 = CARTESIAN_POINT ( 'NONE',  ( 1.735739373471972158, 26.42668463374644361, -1.556826290527684620 ) ) ;
#4065 = CARTESIAN_POINT ( 'NONE',  ( 5.690494692575421176, 14.49221151649372352, 2.273377197464830246 ) ) ;
#4066 = CARTESIAN_POINT ( 'NONE',  ( -2.500000000000000000, 28.23419673618999681, 0.000000000000000000 ) ) ;
#4067 = ADVANCED_FACE ( 'NONE', ( #23712 ), #16533, .F. ) ;
#4068 = CARTESIAN_POINT ( 'NONE',  ( 1.154729593009722333, 30.47563926276945168, 1.826466678455010983 ) ) ;
#4069 = VERTEX_POINT ( 'NONE', #21554 ) ;
#4070 = EDGE_CURVE ( 'NONE', #14850, #18988, #6887, .T. ) ;
#4071 = CARTESIAN_POINT ( 'NONE',  ( 19.59471007437000267, 8.951466053687999747, 3.915631828095000877 ) ) ;
#4072 = CARTESIAN_POINT ( 'NONE',  ( -0.5533348865729804666, 12.81413901064252236, -6.643174729024203806 ) ) ;
#4073 = DIRECTION ( 'NONE',  ( 0.000000000000000000, -1.000000000000000000, -2.763496998553999776E-10 ) ) ;
#4074 = CARTESIAN_POINT ( 'NONE',  ( -22.70605529217283447, -8.531959713363267639, -6.226904222294471936 ) ) ;
#4075 = CARTESIAN_POINT ( 'NONE',  ( -2.459101194521000178, 26.82946440325999760, 0.1450207862197999964 ) ) ;
#4076 = CONICAL_SURFACE ( 'NONE', #23796, 2.249999993254999886, 0.7853981633972997312 ) ;
#4077 = CYLINDRICAL_SURFACE ( 'NONE', #7723, 11.50000000000000000 ) ;
#4078 = ORIENTED_EDGE ( 'NONE', *, *, #2707, .F. ) ;
#4079 = CARTESIAN_POINT ( 'NONE',  ( -17.15404741204965688, -5.529600172785069212, -8.836923940253553766 ) ) ;
#4080 = ADVANCED_FACE ( 'NONE', ( #18167 ), #7248, .T. ) ;
#4081 = FACE_OUTER_BOUND ( 'NONE', #13883, .T. ) ;
#4082 = ADVANCED_FACE ( 'NONE', ( #6766 ), #4967, .T. ) ;
#4083 = CARTESIAN_POINT ( 'NONE',  ( 0.3345823118753548098, 28.21060522079947575, -2.176823781557687187 ) ) ;
#4084 = VERTEX_POINT ( 'NONE', #1570 ) ;
#4085 = CARTESIAN_POINT ( 'NONE',  ( 23.99478584078000054, -6.383504859171999612, 12.40379814865999997 ) ) ;
#4086 = CARTESIAN_POINT ( 'NONE',  ( 18.49162674931000083, 10.23722398798000022, 3.399059637929999766 ) ) ;
#4087 = AXIS2_PLACEMENT_3D ( 'NONE', #4391, #17471, #11782 ) ;
#4088 = CARTESIAN_POINT ( 'NONE',  ( -17.39131617766999938, -8.850658443533001574, -7.172809675466000456 ) ) ;
#4089 = CARTESIAN_POINT ( 'NONE',  ( 23.77835672501372599, -9.281039036324623126, -1.918975276430111748E-05 ) ) ;
#4090 = CARTESIAN_POINT ( 'NONE',  ( 18.17176537305999773, -4.883153369406000088, -9.730320138885000247 ) ) ;
#4091 = CARTESIAN_POINT ( 'NONE',  ( -6.042815982636000172, 21.50000000000000000, -1.000000000000000000 ) ) ;
#4092 = FACE_OUTER_BOUND ( 'NONE', #22033, .T. ) ;
#4093 = CARTESIAN_POINT ( 'NONE',  ( 23.67704510333999579, -9.540510436538999883, -3.867765119376000094 ) ) ;
#4094 = CARTESIAN_POINT ( 'NONE',  ( 23.99999963380662749, 13.93375672974000068, 0.09624782602625137073 ) ) ;
#4095 = VERTEX_POINT ( 'NONE', #8713 ) ;
#4096 = CARTESIAN_POINT ( 'NONE',  ( 12.35781481503000023, 4.416401984941999537, -7.958029298064000834 ) ) ;
#4097 = CARTESIAN_POINT ( 'NONE',  ( -2.804372049896000085, 26.48750240010000212, 0.6153010951427000386 ) ) ;
#4098 = CARTESIAN_POINT ( 'NONE',  ( 0.8375093185100999094, 11.48200882685999780, 4.871193163113003877 ) ) ;
#4099 = CARTESIAN_POINT ( 'NONE',  ( 2.109404096337074375, 29.03140909393173530, -0.4645879857137120150 ) ) ;
#4100 = CARTESIAN_POINT ( 'NONE',  ( -22.93816914322000144, -10.13184090208999955, -4.608035378405999971 ) ) ;
#4101 = ORIENTED_EDGE ( 'NONE', *, *, #5500, .F. ) ;
#4102 = CARTESIAN_POINT ( 'NONE',  ( 4.724999978625000097, 14.90000002138000035, 2.519183602109999904E-09 ) ) ;
#4103 = ORIENTED_EDGE ( 'NONE', *, *, #15455, .F. ) ;
#4104 = CARTESIAN_POINT ( 'NONE',  ( 15.59795603379665074, 4.568490502191478342, -7.926650740716842058 ) ) ;
#4105 = CARTESIAN_POINT ( 'NONE',  ( -2.400843557866978006, 11.81756170137088269, 4.145428949226574566 ) ) ;
#4106 = CARTESIAN_POINT ( 'NONE',  ( 1.831974274068000064, 25.63049822781000131, 0.9334375154566999511 ) ) ;
#4107 = CARTESIAN_POINT ( 'NONE',  ( 1.499999883624000052, 7.099999883624000141, -4.580366257796999989E-07 ) ) ;
#4108 = TOROIDAL_SURFACE ( 'NONE', #20740, 2.500000000000000000, 0.5500000000000000444 ) ;
#4109 = CARTESIAN_POINT ( 'NONE',  ( -8.000000000000000000, 1.322618543078999814E-14, 0.000000000000000000 ) ) ;
#4110 = CARTESIAN_POINT ( 'NONE',  ( 15.09131424931000076, 4.764171260128000185, 9.577928620034999341 ) ) ;
#4111 = CARTESIAN_POINT ( 'NONE',  ( -12.99567423753000028, 6.199143636224999199, -8.762012042742998830 ) ) ;
#4112 = CARTESIAN_POINT ( 'NONE',  ( 24.00016455292000117, -6.692834685703999753, -6.438753808737999407 ) ) ;
#4113 = CARTESIAN_POINT ( 'NONE',  ( 24.07420734439604004, 13.66464621573615190, -1.332138486891153217 ) ) ;
#4114 = ORIENTED_EDGE ( 'NONE', *, *, #4700, .F. ) ;
#4115 = FACE_OUTER_BOUND ( 'NONE', #22570, .T. ) ;
#4116 = AXIS2_PLACEMENT_3D ( 'NONE', #6490, #8434, #13993 ) ;
#4117 = CARTESIAN_POINT ( 'NONE',  ( 0.9856789269715999779, 25.22148090944999765, 2.530880771168000365 ) ) ;
#4118 = CARTESIAN_POINT ( 'NONE',  ( 13.89455729310778942, -9.502394204169668512, 4.016926027372820229 ) ) ;
#4119 = CARTESIAN_POINT ( 'NONE',  ( 0.6559879769048997389, 12.68326117563999667, -7.060560187867004345 ) ) ;
#4120 = SURFACE_STYLE_USAGE ( .BOTH. , #17193 ) ;
#4121 = CARTESIAN_POINT ( 'NONE',  ( 0.2669411416847999874, 28.86629219681999814, -2.539114488640000111 ) ) ;
#4122 = CARTESIAN_POINT ( 'NONE',  ( 11.06626444616512828, 0.2510812432465111543, 12.49999588481644608 ) ) ;
#4123 = DIRECTION ( 'NONE',  ( -1.000000000000000000, 0.000000000000000000, 0.000000000000000000 ) ) ;
#4124 = AXIS2_PLACEMENT_3D ( 'NONE', #17488, #21246, #15648 ) ;
#4125 = DIRECTION ( 'NONE',  ( 0.7071067811880967779, 0.7071067811849969242, -4.142944449020979899E-08 ) ) ;
#4126 = CARTESIAN_POINT ( 'NONE',  ( 0.000000000000000000, 19.00000000000000000, 0.000000000000000000 ) ) ;
#4127 = ORIENTED_EDGE ( 'NONE', *, *, #20478, .T. ) ;
#4128 = CARTESIAN_POINT ( 'NONE',  ( -24.50000000000000000, 0.000000000000000000, -12.50000000000000000 ) ) ;
#4129 = ORIENTED_EDGE ( 'NONE', *, *, #3199, .T. ) ;
#4130 = CARTESIAN_POINT ( 'NONE',  ( 2.410494989090000040, 25.19716278443000235, 1.296714785155999916 ) ) ;
#4131 = CARTESIAN_POINT ( 'NONE',  ( 0.000000000000000000, 23.50000000000000000, 0.000000000000000000 ) ) ;
#4132 = FACE_OUTER_BOUND ( 'NONE', #23776, .T. ) ;
#4133 = ORIENTED_EDGE ( 'NONE', *, *, #18692, .T. ) ;
#4134 = CARTESIAN_POINT ( 'NONE',  ( 13.75702809931000026, -10.56473829713000079, 3.046569488393000125 ) ) ;
#4135 = CARTESIAN_POINT ( 'NONE',  ( -23.76320755544999841, -6.968962349015999536, 12.06578410929999912 ) ) ;
#4136 = AXIS2_PLACEMENT_3D ( 'NONE', #7262, #22050, #22507 ) ;
#4137 = CARTESIAN_POINT ( 'NONE',  ( -2.329463490920999913, 28.34462896666999754, 1.304555153736000062 ) ) ;
#4138 = ORIENTED_EDGE ( 'NONE', *, *, #17780, .F. ) ;
#4139 = VERTEX_POINT ( 'NONE', #14624 ) ;
#4140 = CIRCLE ( 'NONE', #17694, 0.5500000000000001554 ) ;
#4141 = DIRECTION ( 'NONE',  ( 7.994189964398003696E-07, -1.682414072936945643E-07, 0.9999999999996664890 ) ) ;
#4142 = CARTESIAN_POINT ( 'NONE',  ( -10.19248471168999970, -8.520788371486000656, 13.03016121583000064 ) ) ;
#4143 = CARTESIAN_POINT ( 'NONE',  ( 1.750000000000001998, 7.000000000000000888, -0.1151749530721415948 ) ) ;
#4144 = CARTESIAN_POINT ( 'NONE',  ( -4.849997028045999414, 12.54999874207999966, 2.403882053831000161E-08 ) ) ;
#4145 = EDGE_CURVE ( 'NONE', #4287, #17972, #21118, .T. ) ;
#4146 = EDGE_LOOP ( 'NONE', ( #18444, #7488, #18540, #18510 ) ) ;
#4147 = CARTESIAN_POINT ( 'NONE',  ( -24.24498014590000139, -9.840995202723000546, -0.7269391992499000255 ) ) ;
#4148 = CARTESIAN_POINT ( 'NONE',  ( 19.81683333333332797, -3.716106903173100662, 8.461018381044933534 ) ) ;
#4149 = FACE_OUTER_BOUND ( 'NONE', #4950, .T. ) ;
#4150 = CARTESIAN_POINT ( 'NONE',  ( 15.60735436316270253, -7.610950483687727086, 7.015716127438307304 ) ) ;
#4151 = CARTESIAN_POINT ( 'NONE',  ( -18.59345419335999949, 8.208879709517999501, -7.496806360130000790 ) ) ;
#4152 = CARTESIAN_POINT ( 'NONE',  ( 0.5506292728288999516, 30.59193204632999752, -2.290976999470999864 ) ) ;
#4153 = AXIS2_PLACEMENT_3D ( 'NONE', #13039, #192, #15083 ) ;
#4154 = CARTESIAN_POINT ( 'NONE',  ( -17.46454189286000158, -8.119858849493999386, 7.209780893148999503 ) ) ;
#4155 = B_SPLINE_CURVE_WITH_KNOTS ( 'NONE', 3,
 ( #2238, #20652, #9750, #22340, #2481, #4063, #13497, #11693 ),
 .UNSPECIFIED., .F., .F.,
 ( 4, 2, 2, 4 ),
 ( 0.000000000000000000, 0.2499999999999997780, 0.4999999999999995559, 1.000000000000000000 ),
 .UNSPECIFIED. ) ;
#4156 = ADVANCED_FACE ( 'NONE', ( #14396 ), #23492, .F. ) ;
#4157 = CARTESIAN_POINT ( 'NONE',  ( -0.4240070336381018823, 29.57875158174377717, 2.118275460938266797 ) ) ;
#4158 = ORIENTED_EDGE ( 'NONE', *, *, #2148, .F. ) ;
#4159 = VECTOR ( 'NONE', #21288, 1000.000000000000000 ) ;
#4160 = B_SPLINE_CURVE_WITH_KNOTS ( 'NONE', 3,
 ( #5178, #16298, #7096, #14486, #21879, #5288, #10864, #18248, #23801, #57, #20415, #9157, #18598, #9507, #14823, #14601, #10975, #3700 ),
 .UNSPECIFIED., .F., .F.,
 ( 4, 2, 2, 2, 2, 2, 2, 2, 4 ),
 ( 0.000000000000000000, 0.1249999999999999722, 0.2500000000000000000, 0.3750000000000000555, 0.5000000000000001110, 0.6250000000000001110, 0.7500000000000000000, 0.8750000000000000000, 1.000000000000000000 ),
 .UNSPECIFIED. ) ;
#4161 = CARTESIAN_POINT ( 'NONE',  ( -2.047002538946999906, 25.14301022640000127, -0.7667419757990000528 ) ) ;
#4162 = CARTESIAN_POINT ( 'NONE',  ( -17.96465470606060677, -4.640328617862117255, 9.358849047281662337 ) ) ;
#4163 = VERTEX_POINT ( 'NONE', #16078 ) ;
#4164 = DIRECTION ( 'NONE',  ( 0.000000000000000000, 1.000000000000000000, 0.000000000000000000 ) ) ;
#4165 = CARTESIAN_POINT ( 'NONE',  ( -5.553896923315000400, 15.03366893909998581, 2.958514830663998563 ) ) ;
#4166 = DIRECTION ( 'NONE',  ( 0.000000000000000000, -1.000000000000000000, 0.000000000000000000 ) ) ;
#4167 = CARTESIAN_POINT ( 'NONE',  ( 17.03925158531000150, -7.718145806856000490, 6.728824147386999854 ) ) ;
#4168 = VERTEX_POINT ( 'NONE', #21787 ) ;
#4169 = VECTOR ( 'NONE', #21020, 1000.000000000000000 ) ;
#4170 = CARTESIAN_POINT ( 'NONE',  ( 18.38737270046332739, -6.348145805352896076, 6.664696905531276805 ) ) ;
#4171 = DIRECTION ( 'NONE',  ( 0.000000000000000000, 0.000000000000000000, -1.000000000000000000 ) ) ;
#4172 = EDGE_CURVE ( 'NONE', #5160, #15484, #16476, .T. ) ;
#4173 = EDGE_LOOP ( 'NONE', ( #15223, #4270, #10172, #11478 ) ) ;
#4174 = CARTESIAN_POINT ( 'NONE',  ( -7.034000000000000696, -10.69999999999999929, 6.692380538630998849E-10 ) ) ;
#4175 = CARTESIAN_POINT ( 'NONE',  ( 0.000000000000000000, 28.30000000000000071, 0.000000000000000000 ) ) ;
#4176 = CARTESIAN_POINT ( 'NONE',  ( 4.691862310626997434, 12.59647401853998971, 1.107358546619999773 ) ) ;
#4177 = LINE ( 'NONE', #4299, #20717 ) ;
#4178 = CARTESIAN_POINT ( 'NONE',  ( 12.00000000000000178, -0.06551022104711376470, -9.358750515500020128 ) ) ;
#4179 = CARTESIAN_POINT ( 'NONE',  ( 19.33933103379666463, 7.330909640340940392, -5.633988034377063414 ) ) ;
#4180 = PLANE ( 'NONE',  #15425 ) ;
#4181 = LINE ( 'NONE', #20303, #11613 ) ;
#4182 = CARTESIAN_POINT ( 'NONE',  ( 0.8545932710616224171, 26.39685207198635553, -4.125402498422513276 ) ) ;
#4183 = CARTESIAN_POINT ( 'NONE',  ( 2.500000000000000000, 24.40000000000000213, 0.000000000000000000 ) ) ;
#4184 = EDGE_CURVE ( 'NONE', #17924, #9190, #11514, .T. ) ;
#4185 = CARTESIAN_POINT ( 'NONE',  ( 0.9032590285184615153, 30.45886934512990152, 1.961921808037713655 ) ) ;
#4186 = ORIENTED_EDGE ( 'NONE', *, *, #12227, .F. ) ;
#4187 = CARTESIAN_POINT ( 'NONE',  ( 20.36771380861000225, -9.778663773954999527, 0.5067347920774000203 ) ) ;
#4188 = CARTESIAN_POINT ( 'NONE',  ( -0.4177920217811221804, 12.80953346229017242, -6.652087608309179778 ) ) ;
#4189 = DIRECTION ( 'NONE',  ( -1.000000000000000000, 0.000000000000000000, 0.000000000000000000 ) ) ;
#4190 = AXIS2_PLACEMENT_3D ( 'NONE', #2188, #15374, #9701 ) ;
#4191 = CARTESIAN_POINT ( 'NONE',  ( -23.26835916760327905, -2.655106138931690563, 10.24194253716867031 ) ) ;
#4192 = CARTESIAN_POINT ( 'NONE',  ( -1.287118485750000207, 28.29196440325999973, -2.100366574696000299 ) ) ;
#4193 = CARTESIAN_POINT ( 'NONE',  ( 0.000000000000000000, 20.00000000000000000, 0.000000000000000000 ) ) ;
#4194 = ORIENTED_EDGE ( 'NONE', *, *, #13685, .T. ) ;
#4195 = EDGE_CURVE ( 'NONE', #18500, #4867, #10744, .T. ) ;
#4196 = AXIS2_PLACEMENT_3D ( 'NONE', #6385, #8581, #1311 ) ;
#4197 = CARTESIAN_POINT ( 'NONE',  ( -18.88454412025865992, -2.787382164252126593, -10.08993089778954122 ) ) ;
#4198 = CARTESIAN_POINT ( 'NONE',  ( -3.304996520289661177, 29.87418302490023692, 2.710661522857509276 ) ) ;
#4199 = AXIS2_PLACEMENT_3D ( 'NONE', #2510, #3978, #11372 ) ;
#4200 = AXIS2_PLACEMENT_3D ( 'NONE', #21126, #19561, #6706 ) ;
#4201 = DIRECTION ( 'NONE',  ( 0.000000000000000000, 1.000000000000000000, 0.000000000000000000 ) ) ;
#4202 = ORIENTED_EDGE ( 'NONE', *, *, #17493, .T. ) ;
#4203 = EDGE_CURVE ( 'NONE', #22775, #6561, #17037, .T. ) ;
#4204 = VERTEX_POINT ( 'NONE', #18502 ) ;
#4205 = ADVANCED_FACE ( 'NONE', ( #434 ), #12923, .F. ) ;
#4206 = DIRECTION ( 'NONE',  ( 0.000000000000000000, -0.3557256971724915284, 0.9345904067403778548 ) ) ;
#4207 = AXIS2_PLACEMENT_3D ( 'NONE', #2317, #18674, #13574 ) ;
#4208 = CARTESIAN_POINT ( 'NONE',  ( 17.50443924930999984, -10.75095007791999890, -0.4607405056646999841 ) ) ;
#4209 = CARTESIAN_POINT ( 'NONE',  ( -13.73496991422000058, -8.032382890017998989, -7.934146143239000359 ) ) ;
#4210 = CARTESIAN_POINT ( 'NONE',  ( 22.60745833333331589, 5.685348439634987372, -7.398154500763331143 ) ) ;
#4211 = CARTESIAN_POINT ( 'NONE',  ( 14.31239037306000128, -10.28425898052000065, -3.229262266925000180 ) ) ;
#4212 = CARTESIAN_POINT ( 'NONE',  ( 13.50000000000000178, -6.755876297955836662, -6.302790169812603871 ) ) ;
#4213 = DIRECTION ( 'NONE',  ( -1.000000000000000000, 0.000000000000000000, 0.000000000000000000 ) ) ;
#4214 = CARTESIAN_POINT ( 'NONE',  ( 23.49999600117999776, -10.02335684408000027, 2.326734473723000018 ) ) ;
#4215 = VECTOR ( 'NONE', #7239, 1000.000000000000000 ) ;
#4216 = EDGE_CURVE ( 'NONE', #3157, #7720, #14740, .T. ) ;
#4217 = DIRECTION ( 'NONE',  ( -1.511005198495999796E-08, -0.9999999999999997780, -8.997177385936997916E-09 ) ) ;
#4218 = ORIENTED_EDGE ( 'NONE', *, *, #22021, .F. ) ;
#4219 = CARTESIAN_POINT ( 'NONE',  ( 12.66027015143999890, 5.546622252611999926, -7.082799009680999625 ) ) ;
#4220 = CARTESIAN_POINT ( 'NONE',  ( 1.777466727206999941, 26.97500240009999928, -2.254705796085000102 ) ) ;
#4221 = CARTESIAN_POINT ( 'NONE',  ( -1.083921081176000056, 11.48516387305999764, 4.746390725385002618 ) ) ;
#4222 = CARTESIAN_POINT ( 'NONE',  ( 2.122476591467600038, 29.02756187265872256, -0.4001553311762567899 ) ) ;
#4223 = CARTESIAN_POINT ( 'NONE',  ( -22.79154754632999769, -10.12821918160999957, -4.606388536657999744 ) ) ;
#4224 = ORIENTED_EDGE ( 'NONE', *, *, #6447, .F. ) ;
#4225 = CARTESIAN_POINT ( 'NONE',  ( 2.270871215252209030, 18.00000000000000000, 0.000000000000000000 ) ) ;
#4226 = VECTOR ( 'NONE', #21278, 1000.000000000000000 ) ;
#4227 = B_SPLINE_CURVE_WITH_KNOTS ( 'NONE', 3,
 ( #3184, #10451, #10567, #17951, #12264, #23513, #12501, #8872, #23019, #13074 ),
 .UNSPECIFIED., .F., .F.,
 ( 4, 1, 1, 2, 2, 4 ),
 ( 0.000000000000000000, 0.2500000000000011657, 0.3750000000000013323, 0.4375000000000017208, 0.5000000000000019984, 1.000000000000000000 ),
 .UNSPECIFIED. ) ;
#4228 = ORIENTED_EDGE ( 'NONE', *, *, #10961, .F. ) ;
#4229 = FACE_OUTER_BOUND ( 'NONE', #18655, .T. ) ;
#4230 = CARTESIAN_POINT ( 'NONE',  ( -4.143437947609855954, 12.32179185387261100, 2.404511302189828559 ) ) ;
#4231 = CARTESIAN_POINT ( 'NONE',  ( 1.107772814030999919, 25.82549822781000159, -1.978081431919000099 ) ) ;
#4232 = CARTESIAN_POINT ( 'NONE',  ( -0.5536789215616996218, 12.68198336050999231, 7.063110854946003769 ) ) ;
#4233 = CARTESIAN_POINT ( 'NONE',  ( -2.000000000000000000, 30.00000000000000000, 3.464101615137999968 ) ) ;
#4234 = CARTESIAN_POINT ( 'NONE',  ( 13.11693924931000055, 9.054732109491999026, 5.598051111924999823 ) ) ;
#4235 = AXIS2_PLACEMENT_3D ( 'NONE', #4193, #3963, #19205 ) ;
#4236 = EDGE_CURVE ( 'NONE', #10806, #12888, #2328, .T. ) ;
#4237 = EDGE_CURVE ( 'NONE', #15884, #16101, #8813, .T. ) ;
#4238 = CARTESIAN_POINT ( 'NONE',  ( -16.00187137585000130, 9.645521962609000965, 3.562832264799999926 ) ) ;
#4239 = AXIS2_PLACEMENT_3D ( 'NONE', #21688, #8487, #1457 ) ;
#4240 = CARTESIAN_POINT ( 'NONE',  ( 17.09606375731000227, -3.490954664894000192, -8.536518206589999380 ) ) ;
#4241 = AXIS2_PLACEMENT_3D ( 'NONE', #16181, #5069, #9161 ) ;
#4242 = DIRECTION ( 'NONE',  ( 0.000000000000000000, 0.000000000000000000, -1.000000000000000000 ) ) ;
#4243 = ORIENTED_EDGE ( 'NONE', *, *, #22670, .T. ) ;
#4244 = CARTESIAN_POINT ( 'NONE',  ( -1.089863560591000091, 30.60758970965000003, 2.496295939784000328 ) ) ;
#4245 = CARTESIAN_POINT ( 'NONE',  ( -2.393157034060999777, 24.23821659520999816, -0.8070405077446000108 ) ) ;
#4246 = CARTESIAN_POINT ( 'NONE',  ( 4.778395690722049061, 14.77598124633097498, -3.832701201829089577 ) ) ;
#4247 = ORIENTED_EDGE ( 'NONE', *, *, #1393, .T. ) ;
#4248 = LINE ( 'NONE', #22994, #14501 ) ;
#4249 = CARTESIAN_POINT ( 'NONE',  ( 20.71127131372000107, 7.811385099584000180, 8.041652894164000642 ) ) ;
#4250 = ADVANCED_FACE ( 'NONE', ( #18382 ), #3851, .T. ) ;
#4251 = CARTESIAN_POINT ( 'NONE',  ( 14.40078967323709946, -4.362328053288525354, 7.919021186112042088 ) ) ;
#4252 = EDGE_CURVE ( 'NONE', #7057, #3560, #13819, .T. ) ;
#4253 = CARTESIAN_POINT ( 'NONE',  ( 18.21132320931108239, 9.336834288664581649, -4.723061267702502342 ) ) ;
#4254 = CARTESIAN_POINT ( 'NONE',  ( 0.000000000000000000, 14.95000002005000006, 0.000000000000000000 ) ) ;
#4255 = CARTESIAN_POINT ( 'NONE',  ( -6.638602398571264551, 15.38275018475912326, 1.627931652404663199 ) ) ;
#4256 = CARTESIAN_POINT ( 'NONE',  ( -9.000000000000000000, 22.00000000000000000, 1.000000000000000000 ) ) ;
#4257 = ORIENTED_EDGE ( 'NONE', *, *, #20883, .F. ) ;
#4258 = CARTESIAN_POINT ( 'NONE',  ( 30.87226923053214378, 37.01856778792605240, 0.000000000000000000 ) ) ;
#4259 = VERTEX_POINT ( 'NONE', #5435 ) ;
#4260 = CYLINDRICAL_SURFACE ( 'NONE', #17265, 0.9999999999999991118 ) ;
#4262 = CARTESIAN_POINT ( 'NONE',  ( -2.500000000000000000, 24.00000000000000000, 8.181116922990998136E-14 ) ) ;
#4261 = LINE ( 'NONE', #22183, #15440 ) ;
#4263 = B_SPLINE_CURVE_WITH_KNOTS ( 'NONE', 3,
 ( #18105, #8902, #7298, #22082, #14571, #20035, #3453, #10837, #21963, #5378, #20155, #12870, #18448, #3794, #16622, #1975, #5149, #7415, #5606, #12986, #18571, #614, #2443, #8018, #20508, #6197, #3915, #18795, #15391, #4387, #17340, #22779 ),
 .UNSPECIFIED., .F., .F.,
 ( 4, 2, 2, 2, 2, 2, 2, 2, 2, 2, 2, 2, 2, 2, 2, 4 ),
 ( 0.000000000000000000, 0.1249999999999978351, 0.1874999999999967526, 0.2187499999999963363, 0.2499999999999959477, 0.3124999999999953371, 0.3437499999999952816, 0.3749999999999951705, 0.4999999999999955591, 0.5624999999999955591, 0.5937499999999956701, 0.6249999999999957812, 0.6874999999999963363, 0.7187499999999965583, 0.7499999999999967804, 1.000000000000000000 ),
 .UNSPECIFIED. ) ;
#4264 = LINE ( 'NONE', #8007, #18846 ) ;
#4265 = AXIS2_PLACEMENT_3D ( 'NONE', #176, #17137, #7698 ) ;
#4266 = CARTESIAN_POINT ( 'NONE',  ( 16.03523116938000115, -10.52587742755999933, -3.387995920261000382 ) ) ;
#4267 = CARTESIAN_POINT ( 'NONE',  ( -6.595625688791005636, 15.16860556014002448, -2.934141294233998387 ) ) ;
#4268 = CARTESIAN_POINT ( 'NONE',  ( 24.15736593520906794, -5.143174366503609818, -12.50000000000000355 ) ) ;
#4269 = VERTEX_POINT ( 'NONE', #20320 ) ;
#4270 = ORIENTED_EDGE ( 'NONE', *, *, #7181, .F. ) ;
#4271 = CARTESIAN_POINT ( 'NONE',  ( -23.99212502900741129, 8.254180775344659438, -10.70333952224147112 ) ) ;
#4272 = CARTESIAN_POINT ( 'NONE',  ( -24.50000000000000000, 1.524685264937999788E-14, 0.000000000000000000 ) ) ;
#4273 = DIRECTION ( 'NONE',  ( 0.000000000000000000, 1.000000000000000000, 0.000000000000000000 ) ) ;
#4274 = EDGE_LOOP ( 'NONE', ( #18213, #19572, #83 ) ) ;
#4275 = CARTESIAN_POINT ( 'NONE',  ( -23.78800218427999980, 0.9048305059418999541, -10.21290675204000031 ) ) ;
#4276 = CARTESIAN_POINT ( 'NONE',  ( -14.47158024777374763, 9.790304928774279603, 8.042633409149424040 ) ) ;
#4277 = CARTESIAN_POINT ( 'NONE',  ( 6.179554688491347036, 13.96940086483144228, 0.6559343789280690507 ) ) ;
#4278 = CARTESIAN_POINT ( 'NONE',  ( 15.58288198016115444, -6.969638865288424689, 7.648956436886991561 ) ) ;
#4279 = CARTESIAN_POINT ( 'NONE',  ( -14.22349291444999864, -7.631317991244999988, 7.918878983168999852 ) ) ;
#4280 = CARTESIAN_POINT ( 'NONE',  ( -1.876762163929999838, 29.36394619264999761, -1.125344217945999814 ) ) ;
#4281 = CARTESIAN_POINT ( 'NONE',  ( -21.66813167847034194, -2.121835831585393795, 10.44917271204820253 ) ) ;
#4282 = CARTESIAN_POINT ( 'NONE',  ( -16.85515084895999749, -2.006433207287000364, -10.65451757797000099 ) ) ;
#4283 = CARTESIAN_POINT ( 'NONE',  ( 1.512189683744231905, 29.70242366392465527, 1.543056007447467737 ) ) ;
#4284 = ORIENTED_EDGE ( 'NONE', *, *, #8942, .F. ) ;
#4285 = CARTESIAN_POINT ( 'NONE',  ( -1.447949418204000027, 25.10653475033999982, -1.849518100036999790 ) ) ;
#4286 = CARTESIAN_POINT ( 'NONE',  ( -19.49843092002534917, -10.39128334678671450, 1.480522605369253286 ) ) ;
#4287 = VERTEX_POINT ( 'NONE', #7356 ) ;
#4288 = ADVANCED_FACE ( 'NONE', ( #18857 ), #19233, .T. ) ;
#4289 = CARTESIAN_POINT ( 'NONE',  ( -2.500000000000000000, 27.43419673618999965, 0.000000000000000000 ) ) ;
#4290 = CARTESIAN_POINT ( 'NONE',  ( -19.72972087121333118, 7.339100371923414023, -5.639965138420785173 ) ) ;
#4291 = CARTESIAN_POINT ( 'NONE',  ( 13.94156392131000111, 3.761510884484999817, -8.885545664707001023 ) ) ;
#4292 = ORIENTED_EDGE ( 'NONE', *, *, #912, .F. ) ;
#4293 = CARTESIAN_POINT ( 'NONE',  ( -6.234717296507000128, 15.63949533431998873, -1.260321238843998604 ) ) ;
#4294 = CARTESIAN_POINT ( 'NONE',  ( 23.99062354302999722, 7.716878364870000340, 11.63397459621999985 ) ) ;
#4295 = EDGE_LOOP ( 'NONE', ( #12553, #12999 ) ) ;
#4296 = CARTESIAN_POINT ( 'NONE',  ( 0.000000000000000000, 20.05000017415440183, -3.049999825846000157 ) ) ;
#4297 = CARTESIAN_POINT ( 'NONE',  ( 21.96499999999999986, -9.234946903777000671, 0.000000000000000000 ) ) ;
#4298 = CARTESIAN_POINT ( 'NONE',  ( -3.981022404528000269, 12.34392304552999597, 2.724439042342001294 ) ) ;
#4299 = CARTESIAN_POINT ( 'NONE',  ( -12.25000000000000000, -13.93375672974000068, 0.000000000000000000 ) ) ;
#4300 = CARTESIAN_POINT ( 'NONE',  ( 18.30891208659113545, 7.138339280091794414, -7.593585127964508352 ) ) ;
#4301 = CARTESIAN_POINT ( 'NONE',  ( -23.75391653307000084, 7.466983940307000189, 11.77825120950999960 ) ) ;
#4302 = FACE_OUTER_BOUND ( 'NONE', #11346, .T. ) ;
#4303 = DIRECTION ( 'NONE',  ( 1.000000000000000000, 0.000000000000000000, 0.000000000000000000 ) ) ;
#4304 = CARTESIAN_POINT ( 'NONE',  ( -4.724999978625000097, 14.90000002138000035, -2.519184009061999785E-09 ) ) ;
#4305 =( LENGTH_UNIT ( ) NAMED_UNIT ( * ) SI_UNIT ( .MILLI., .METRE. ) );
#4306 = CARTESIAN_POINT ( 'NONE',  ( 1.750000000000000000, 7.000000000000000000, 0.000000000000000000 ) ) ;
#4307 = CARTESIAN_POINT ( 'NONE',  ( 0.9439321425118507580, 30.46150519779229526, 1.942806962222955791 ) ) ;
#4308 = ORIENTED_EDGE ( 'NONE', *, *, #15366, .T. ) ;
#4309 = CARTESIAN_POINT ( 'NONE',  ( 20.94746660927999926, 3.688233682878999886, -9.087913520545999546 ) ) ;
#4310 = CARTESIAN_POINT ( 'NONE',  ( 1.231503247170836257, 12.85502785828538919, -6.563768214206104012 ) ) ;
#4311 = CARTESIAN_POINT ( 'NONE',  ( -23.50032910583999879, -5.270462733209999584, -7.631233524726999562 ) ) ;
#4312 = EDGE_CURVE ( 'NONE', #7164, #15500, #23428, .T. ) ;
#4313 = CARTESIAN_POINT ( 'NONE',  ( -19.57321941476413940, -4.900126282342609940, 9.269928300904794582 ) ) ;
#4314 = CARTESIAN_POINT ( 'NONE',  ( 1.419229835182000077, 26.50364211381999979, -1.800284464616000113 ) ) ;
#4315 = CARTESIAN_POINT ( 'NONE',  ( -3.824747491000654698, 24.75094615491947891, -2.410583160005970171 ) ) ;
#4316 = ORIENTED_EDGE ( 'NONE', *, *, #21183, .T. ) ;
#4317 = CARTESIAN_POINT ( 'NONE',  ( -17.54480473325896028, -9.830998375515614285, 3.491180853190327227 ) ) ;
#4318 = DIRECTION ( 'NONE',  ( 0.8500000000000165201, 0.000000000000000000, -0.5267826876426102700 ) ) ;
#4319 = CARTESIAN_POINT ( 'NONE',  ( 0.000000000000000000, 20.05000017415440183, 0.000000000000000000 ) ) ;
#4320 = APPLICATION_CONTEXT ( 'automotive_design' ) ;
#4321 = ORIENTED_EDGE ( 'NONE', *, *, #9786, .F. ) ;
#4322 = EDGE_CURVE ( 'NONE', #6372, #11438, #22241, .T. ) ;
#4323 = ORIENTED_EDGE ( 'NONE', *, *, #12648, .T. ) ;
#4324 = CARTESIAN_POINT ( 'NONE',  ( -4.820912286398000290, 1.283685947151999869E-14, 0.000000000000000000 ) ) ;
#4325 = CARTESIAN_POINT ( 'NONE',  ( 11.99362658531000037, -8.009633343651000104, -6.163949985837000156 ) ) ;
#4326 = CARTESIAN_POINT ( 'NONE',  ( -15.96940374187999900, -8.848765849800999561, 7.112061138617000289 ) ) ;
#4327 = FACE_OUTER_BOUND ( 'NONE', #15145, .T. ) ;
#4328 = CARTESIAN_POINT ( 'NONE',  ( 16.47858580085999947, 8.864729889898001147, -7.134999139258999534 ) ) ;
#4329 = DIRECTION ( 'NONE',  ( -1.000000000000000000, 0.000000000000000000, 0.000000000000000000 ) ) ;
#4330 = CARTESIAN_POINT ( 'NONE',  ( -0.6543697108981785249, 28.96666666666666501, 2.434931691670795484 ) ) ;
#4331 = CARTESIAN_POINT ( 'NONE',  ( 19.42786665163000137, 1.857528855125000211, 9.378182122424998823 ) ) ;
#4332 = VECTOR ( 'NONE', #13729, 1000.000000000000000 ) ;
#4333 = CARTESIAN_POINT ( 'NONE',  ( -2.381850618623087001, 26.58949608044243718, -0.8771401830057823368 ) ) ;
#4334 = ORIENTED_EDGE ( 'NONE', *, *, #10576, .T. ) ;
#4335 = CARTESIAN_POINT ( 'NONE',  ( -23.74465998031000069, 7.716878364870000340, -11.63397459621999985 ) ) ;
#4336 = CARTESIAN_POINT ( 'NONE',  ( 2.554499528901000183, 25.99206776952000197, -0.7744564004552999537 ) ) ;
#4337 = CARTESIAN_POINT ( 'NONE',  ( 3.918384635635002500, 12.23938247889000763, 2.649806649680000348 ) ) ;
#4338 = CARTESIAN_POINT ( 'NONE',  ( 2.050298679598668183, 28.96300717529661028, 0.6792431909432838921 ) ) ;
#4339 = EDGE_CURVE ( 'NONE', #2252, #17770, #8435, .T. ) ;
#4340 = CARTESIAN_POINT ( 'NONE',  ( -23.60650732633999738, 3.478347009544000112, 10.59213551982000112 ) ) ;
#4341 = ORIENTED_EDGE ( 'NONE', *, *, #5144, .T. ) ;
#4342 = DIRECTION ( 'NONE',  ( 0.000000000000000000, 1.000000000000000000, 0.000000000000000000 ) ) ;
#4343 = ORIENTED_EDGE ( 'NONE', *, *, #7592, .F. ) ;
#4344 = CARTESIAN_POINT ( 'NONE',  ( 0.000000000000000000, -1.550000000000000044, 0.000000000000000000 ) ) ;
#4345 = CARTESIAN_POINT ( 'NONE',  ( 0.5271288625574210851, 26.26111511314614688, 2.095841999210956264 ) ) ;
#4346 = DIRECTION ( 'NONE',  ( 0.000000000000000000, 1.000000000000000000, 0.000000000000000000 ) ) ;
#4347 = CARTESIAN_POINT ( 'NONE',  ( -0.5078543351473996381, 12.73453039277000975, 6.462334485033003340 ) ) ;
#4348 = CARTESIAN_POINT ( 'NONE',  ( 0.8157680887313131235, 6.826070574582712602, 1.551609257856797930 ) ) ;
#4349 = CARTESIAN_POINT ( 'NONE',  ( 13.00725174931000083, 10.48226630763000067, 1.840397312871999924 ) ) ;
#4350 = EDGE_CURVE ( 'NONE', #2621, #20340, #14969, .T. ) ;
#4351 = CARTESIAN_POINT ( 'NONE',  ( -17.05828119693000033, -8.427367219174998425, -6.829844779585000580 ) ) ;
#4352 = AXIS2_PLACEMENT_3D ( 'NONE', #1945, #18762, #1826 ) ;
#4353 = CARTESIAN_POINT ( 'NONE',  ( 15.01200125731000057, -8.889299820566000321, -2.243156938537000045 ) ) ;
#4354 = CARTESIAN_POINT ( 'NONE',  ( 0.000000000000000000, 20.00000000000000000, 0.000000000000000000 ) ) ;
#4355 = ORIENTED_EDGE ( 'NONE', *, *, #14435, .T. ) ;
#4356 = CARTESIAN_POINT ( 'NONE',  ( 1.600110441081000090, 30.73994915060000110, 2.204300939401000026 ) ) ;
#4357 = CARTESIAN_POINT ( 'NONE',  ( -1.707744019578999906, 24.17417548081000334, -1.860678729632000206 ) ) ;
#4358 = CARTESIAN_POINT ( 'NONE',  ( 14.19128063372930093, -8.307842784655305124, -6.108522269369860425 ) ) ;
#4359 = CARTESIAN_POINT ( 'NONE',  ( 4.859204854983003585, 14.34044420429000688, -3.623738212790001967 ) ) ;
#4360 = CARTESIAN_POINT ( 'NONE',  ( -23.86847083086766474, 13.66493546065227349, -1.331637500005085073 ) ) ;
#4361 = CARTESIAN_POINT ( 'NONE',  ( 1.600279783570000003, 30.05341750703000159, 2.231095953505000118 ) ) ;
#4362 = CARTESIAN_POINT ( 'NONE',  ( -3.100000000000000089, 20.00000000000000000, 0.000000000000000000 ) ) ;
#4363 = CARTESIAN_POINT ( 'NONE',  ( 0.000000000000000000, 21.89999999999999858, 0.000000000000000000 ) ) ;
#4364 = DIRECTION ( 'NONE',  ( 0.000000000000000000, 0.000000000000000000, 1.000000000000000000 ) ) ;
#4365 = CYLINDRICAL_SURFACE ( 'NONE', #15806, 5.000000000000000000 ) ;
#4366 = ADVANCED_FACE ( 'NONE', ( #13165 ), #22321, .F. ) ;
#4367 = CARTESIAN_POINT ( 'NONE',  ( 2.500000000000000000, 29.45086340285666537, -0.3272492347489373565 ) ) ;
#4368 = ORIENTED_EDGE ( 'NONE', *, *, #4237, .T. ) ;
#4369 = EDGE_CURVE ( 'NONE', #2983, #20057, #11894, .T. ) ;
#4370 = B_SPLINE_CURVE_WITH_KNOTS ( 'NONE', 3,
 ( #19770, #23509, #16352, #14423, #19999, #14535, #6793, #16239, #19882, #3421 ),
 .UNSPECIFIED., .F., .F.,
 ( 4, 2, 2, 2, 4 ),
 ( 0.000000000000000000, 0.2500000000000000555, 0.5000000000000001110, 0.7500000000000000000, 1.000000000000000000 ),
 .UNSPECIFIED. ) ;
#4371 = CIRCLE ( 'NONE', #11332, 2.100000000000000089 ) ;
#4372 = CARTESIAN_POINT ( 'NONE',  ( 11.36448692219539680, -12.20430913922039906, 3.861467675482649131 ) ) ;
#4373 = EDGE_LOOP ( 'NONE', ( #12942, #12279, #8611, #15844, #7582, #15139 ) ) ;
#4374 = B_SPLINE_SURFACE_WITH_KNOTS ( 'NONE', 3, 3, ( 
 ( #3490, #16770, #14722, #10870, #179, #18255, #7570, #1657, #18365, #22119, #9046, #21773, #7217, #19955, #3374, #10753, #1550, #1776, #10153, #20810, #17539, #447, #934, #4220, #7970, #15341, #13769, #22614, #4097, #19228, #8332, #15699, #8099, #816, #11612 ),
 ( #15466, #2394, #2768, #18983, #23088, #563, #2513, #22852, #9783, #6265, #22731, #8216, #11849, #2642, #6513, #17049, #20688, #17169, #11493, #7850, #18870, #6145, #13534, #20930, #21171, #6023, #2275, #10037, #9668, #15217, #13649, #15583, #4336, #13409, #11728 ),
 ( #17422, #21046, #4458, #19362, #19102, #9904, #17291, #693, #22970, #6386, #4583, #11974, #1433, #19481, #8941, #4953, #12097, #16065, #12459, #16190, #23591, #21778, #12338, #4829, #19842, #23701, #12572, #23337, #6995, #14384, #19730, #21664, #1059, #8582, #15943 ),
 ( #6633, #3141, #18027, #2891, #5190, #8460, #19960, #5077, #8700, #21414, #6752, #14145, #21540, #3379, #10760, #3012, #10525, #23462, #10271, #12214, #17908, #8828, #21299, #19604, #1312, #15827, #18153, #1557, #6874, #10399, #17791, #14266, #3255, #14023, #16309 ) ),
 .UNSPECIFIED., .F., .F., .F.,
 ( 4, 4 ),
 ( 4, 1, 1, 1, 1, 1, 1, 1, 1, 1, 1, 1, 1, 1, 1, 1, 1, 1, 1, 1, 1, 1, 1, 1, 1, 1, 1, 1, 1, 1, 1, 1, 4 ),
 ( -0.3056682515952000023, 1.305668251594999996 ),
 ( -0.02000000000000000042, 0.01250000000000000069, 0.04499999999999999833, 0.07749999999999999944, 0.1100000000000000006, 0.1424999999999999878, 0.1749999999999999889, 0.2074999999999999900, 0.2399999999999999911, 0.2725000000000000200, 0.3049999999999999933, 0.3375000000000000222, 0.3699999999999999956, 0.4025000000000000244, 0.4349999999999999978, 0.4675000000000000266, 0.5000000000000000000, 0.5324999999999999734, 0.5649999999999999467, 0.5975000000000000311, 0.6300000000000000044, 0.6624999999999999778, 0.6949999999999999512, 0.7275000000000000355, 0.7600000000000000089, 0.7924999999999999822, 0.8249999999999999556, 0.8575000000000000400, 0.8900000000000000133, 0.9224999999999999867, 0.9549999999999999600, 0.9875000000000000444, 1.020000000000000018 ),
 .UNSPECIFIED. ) ;
#4375 = CARTESIAN_POINT ( 'NONE',  ( -5.759369968430410935, 16.25388642460873356, -2.084701305734063315 ) ) ;
#4377 = CARTESIAN_POINT ( 'NONE',  ( 0.4070492355296851938, 24.37989684473771845, -2.155747726877813797 ) ) ;
#4376 = CARTESIAN_POINT ( 'NONE',  ( -2.017784670879433140, 11.65584428263783145, 4.375368794292053387 ) ) ;
#4378 = CARTESIAN_POINT ( 'NONE',  ( -1.306994031390691813, 29.96241504948190126, -3.864208797664316020 ) ) ;
#4379 = CARTESIAN_POINT ( 'NONE',  ( 14.05027129307999978, -10.57245532834000024, 3.048794078394999829 ) ) ;
#4380 = DIRECTION ( 'NONE',  ( -0.000000000000000000, 1.000000000000000000, 0.000000000000000000 ) ) ;
#4381 = CARTESIAN_POINT ( 'NONE',  ( -1.200923599098000061, 26.50000000000000000, 5.906307787036999990 ) ) ;
#4382 = ADVANCED_FACE ( 'NONE', ( #10259 ), #1461, .T. ) ;
#4383 = EDGE_LOOP ( 'NONE', ( #20928, #11277, #12848, #3911 ) ) ;
#4384 = ORIENTED_EDGE ( 'NONE', *, *, #10887, .F. ) ;
#4385 = CARTESIAN_POINT ( 'NONE',  ( -14.00000000000000000, 1.129711127297478246, -9.368077886284350342 ) ) ;
#4386 = DIRECTION ( 'NONE',  ( 0.000000000000000000, -1.000000000000000000, 0.000000000000000000 ) ) ;
#4387 = CARTESIAN_POINT ( 'NONE',  ( -14.39391696178579494, -8.762017990471466788, -9.823718642519271071 ) ) ;
#4388 = ORIENTED_EDGE ( 'NONE', *, *, #808, .T. ) ;
#4389 = CARTESIAN_POINT ( 'NONE',  ( 2.653270836322024984, 28.03198827073824617, -3.086600612158303392 ) ) ;
#4390 = AXIS2_PLACEMENT_3D ( 'NONE', #8983, #23856, #3758 ) ;
#4391 = CARTESIAN_POINT ( 'NONE',  ( 0.000000000000000000, 22.00000000000000000, 0.000000000000000000 ) ) ;
#4392 = CARTESIAN_POINT ( 'NONE',  ( 15.58582384231821294, -7.050459548571376800, 7.574867977535271635 ) ) ;
#4393 = B_SPLINE_CURVE_WITH_KNOTS ( 'NONE', 3,
 ( #134, #20968, #4017, #4378, #13100, #19023, #17207, #18909, #22649, #7523 ),
 .UNSPECIFIED., .F., .F.,
 ( 4, 1, 1, 2, 2, 4 ),
 ( 0.000000000000000000, 0.2499999999999994449, 0.3749999999999994449, 0.4375000000000000000, 0.5000000000000005551, 1.000000000000000000 ),
 .UNSPECIFIED. ) ;
#4394 = CARTESIAN_POINT ( 'NONE',  ( -15.30747280464999882, 1.690426505166000126, -10.89665494706000004 ) ) ;
#4395 = CARTESIAN_POINT ( 'NONE',  ( 1.835060406389813270, 24.49999999999984368, 3.559329533908949461 ) ) ;
#4396 = CARTESIAN_POINT ( 'NONE',  ( -20.69019690006062717, 4.549517228506217315, -9.473981616376564219 ) ) ;
#4397 = AXIS2_PLACEMENT_3D ( 'NONE', #20179, #167, #20413 ) ;
#4398 = B_SPLINE_CURVE_WITH_KNOTS ( 'NONE', 3,
 ( #12831, #20225, #3981, #212, #9196, #9549, #1808, #16927, #7369, #9315, #14868, #14754, #7605, #22150, #14984, #22381 ),
 .UNSPECIFIED., .F., .F.,
 ( 4, 2, 2, 1, 1, 2, 2, 2, 4 ),
 ( 0.000000000000000000, 0.1249999999999998057, 0.2499999999999996114, 0.3749999999999994449, 0.4374999999999993339, 0.4687499999999993339, 0.4999999999999993339, 0.7499999999999995559, 1.000000000000000000 ),
 .UNSPECIFIED. ) ;
#4399 = CARTESIAN_POINT ( 'NONE',  ( -12.61636557635000067, 8.538192823868000048, -4.467067395255999607 ) ) ;
#4400 = CARTESIAN_POINT ( 'NONE',  ( -1.507258510594286616, 29.50557409157621436, 1.546987692870358089 ) ) ;
#4401 = EDGE_LOOP ( 'NONE', ( #3077, #14503, #23367, #14633 ) ) ;
#4402 = CARTESIAN_POINT ( 'NONE',  ( -18.36980313993808522, 8.462731522496705239, 6.141897997985012125 ) ) ;
#4403 = ORIENTED_EDGE ( 'NONE', *, *, #627, .F. ) ;
#4404 = CARTESIAN_POINT ( 'NONE',  ( 5.512521265958003625, 13.91027821615000093, -3.003820387280002446 ) ) ;
#4405 = CARTESIAN_POINT ( 'NONE',  ( -12.50000000000000000, 6.965460728298000781, -5.686777139159000072 ) ) ;
#4406 = AXIS2_PLACEMENT_3D ( 'NONE', #22894, #12018, #21336 ) ;
#4407 = CARTESIAN_POINT ( 'NONE',  ( 17.91675158530999923, 7.007286630565999985, -7.497846106583000214 ) ) ;
#4408 = ORIENTED_EDGE ( 'NONE', *, *, #11941, .T. ) ;
#4409 = CARTESIAN_POINT ( 'NONE',  ( 18.28712270046333899, -3.700215461176396659, 8.424836998218975026 ) ) ;
#4410 = CARTESIAN_POINT ( 'NONE',  ( 0.6543697108981982868, 26.96666666666666501, -2.434931691670790155 ) ) ;
#4411 = CARTESIAN_POINT ( 'NONE',  ( -6.637070260807000466, 28.00000000000000000, 2.000000000000000000 ) ) ;
#4412 = ORIENTED_EDGE ( 'NONE', *, *, #12950, .T. ) ;
#4413 = CIRCLE ( 'NONE', #17968, 12.38248359579000279 ) ;
#4414 = CARTESIAN_POINT ( 'NONE',  ( -1.670832290882946713, 24.71086476070425419, 1.427778279994880606 ) ) ;
#4415 = B_SPLINE_CURVE_WITH_KNOTS ( 'NONE', 3,
 ( #22622, #2652, #13298, #20939 ),
 .UNSPECIFIED., .F., .F.,
 ( 4, 4 ),
 ( 0.000000000000000000, 1.000000000000000000 ),
 .UNSPECIFIED. ) ;
#4416 = CARTESIAN_POINT ( 'NONE',  ( -9.000000000000000000, 24.99999999999999645, 1.000000000000000000 ) ) ;
#4417 = VECTOR ( 'NONE', #21401, 1000.000000000000000 ) ;
#4418 = CARTESIAN_POINT ( 'NONE',  ( 0.000000000000000000, 19.00000000000000000, 0.000000000000000000 ) ) ;
#4419 = DIRECTION ( 'NONE',  ( -0.9996708941621513800, -0.02565352539212875996, 2.352933579521886060E-14 ) ) ;
#4420 = CARTESIAN_POINT ( 'NONE',  ( 17.66271362385008104, -10.35725960301209092, -0.9534308961195087084 ) ) ;
#4421 = DIRECTION ( 'NONE',  ( -1.000000000000000000, 0.000000000000000000, 0.000000000000000000 ) ) ;
#4422 = CYLINDRICAL_SURFACE ( 'NONE', #13383, 10.59999999999999964 ) ;
#4423 = CARTESIAN_POINT ( 'NONE',  ( 19.86738723104999949, 5.001395480264999804, -10.00765157440999964 ) ) ;
#4424 = DIRECTION ( 'NONE',  ( 0.000000000000000000, -1.000000000000000000, 0.000000000000000000 ) ) ;
#4425 = CARTESIAN_POINT ( 'NONE',  ( 2.500000000000000000, 28.63419673618999894, 0.000000000000000000 ) ) ;
#4426 = CARTESIAN_POINT ( 'NONE',  ( -4.750000000000000000, 22.00000000000000000, 0.000000000000000000 ) ) ;
#4427 = CARTESIAN_POINT ( 'NONE',  ( -0.6004538078361787434, 30.36805637628708610, 2.074802447086620649 ) ) ;
#4428 = ORIENTED_EDGE ( 'NONE', *, *, #5244, .F. ) ;
#4429 = CARTESIAN_POINT ( 'NONE',  ( -16.71228743917333759, -7.277179538279706428, 5.592378764700831617 ) ) ;
#4430 = CARTESIAN_POINT ( 'NONE',  ( 19.64727180480999991, 9.968845625174999725, -2.620031903844999732 ) ) ;
#4431 = CARTESIAN_POINT ( 'NONE',  ( 1.073567819982733207, 12.84232628255067965, -6.588562543359082646 ) ) ;
#4432 = DIRECTION ( 'NONE',  ( 0.000000000000000000, 0.000000000000000000, -1.000000000000000000 ) ) ;
#4433 = DIRECTION ( 'NONE',  ( 0.000000000000000000, 1.000000000000000000, 0.000000000000000000 ) ) ;
#4434 = CARTESIAN_POINT ( 'NONE',  ( 1.992911166421000191, 26.34196440326000044, 1.447934651311999943 ) ) ;
#4435 = CARTESIAN_POINT ( 'NONE',  ( -4.900699999999999612, 1.284663064832999817E-14, 0.000000000000000000 ) ) ;
#4436 = ORIENTED_EDGE ( 'NONE', *, *, #8654, .F. ) ;
#4437 = CARTESIAN_POINT ( 'NONE',  ( -18.38214185013208990, 10.40616288478918250, -1.044753050767677438 ) ) ;
#4438 = CARTESIAN_POINT ( 'NONE',  ( -9.000000000000000000, 18.50000000000000000, -2.000000000000000000 ) ) ;
#4439 = AXIS2_PLACEMENT_3D ( 'NONE', #5223, #16097, #21921 ) ;
#4440 = CARTESIAN_POINT ( 'NONE',  ( 2.059621423746683888, 27.98870470916865472, 0.6859841289820139965 ) ) ;
#4441 = DIRECTION ( 'NONE',  ( 0.000000000000000000, 0.000000000000000000, 1.000000000000000000 ) ) ;
#4442 = ORIENTED_EDGE ( 'NONE', *, *, #8066, .F. ) ;
#4443 = VERTEX_POINT ( 'NONE', #4569 ) ;
#4444 = DIRECTION ( 'NONE',  ( -1.000000000000000000, 0.000000000000000000, 0.000000000000000000 ) ) ;
#4445 = VECTOR ( 'NONE', #12429, 1000.000000000000114 ) ;
#4446 = CARTESIAN_POINT ( 'NONE',  ( 14.32350174931000097, 0.2192049860668999761, -10.67495121044000150 ) ) ;
#4447 = CARTESIAN_POINT ( 'NONE',  ( -14.50244144996998408, -6.856859659331884238, -5.968632047789297346 ) ) ;
#4448 = EDGE_CURVE ( 'NONE', #22775, #23793, #15120, .T. ) ;
#4449 = CARTESIAN_POINT ( 'NONE',  ( -18.61009826548999868, 10.52931532496999978, -4.437563658045000636 ) ) ;
#4450 = LINE ( 'NONE', #438, #19299 ) ;
#4451 = CARTESIAN_POINT ( 'NONE',  ( 17.29249951746000136, 7.620899816286000217, -6.134110199842999656 ) ) ;
#4452 = FACE_OUTER_BOUND ( 'NONE', #4992, .T. ) ;
#4453 = DIRECTION ( 'NONE',  ( -1.000000000000000000, 0.000000000000000000, 0.000000000000000000 ) ) ;
#4454 = CARTESIAN_POINT ( 'NONE',  ( 22.70900596046000075, 7.018910044166999818, -6.751668252317999830 ) ) ;
#4455 = CARTESIAN_POINT ( 'NONE',  ( -1.940710640446570823, 26.54479542469487185, -1.635918543245983070 ) ) ;
#4456 = ORIENTED_EDGE ( 'NONE', *, *, #22088, .T. ) ;
#4457 = CARTESIAN_POINT ( 'NONE',  ( 1.719681894094051477, 13.83405848052206544, 5.882549610230969783 ) ) ;
#4458 = CARTESIAN_POINT ( 'NONE',  ( -0.7160459369171999766, 28.81163313895000044, 2.361836001938000251 ) ) ;
#4459 = AXIS2_PLACEMENT_3D ( 'NONE', #23240, #17930, #15965 ) ;
#4460 = CARTESIAN_POINT ( 'NONE',  ( -4.368769711663002653, 12.39958269994001405, 1.811125832054002460 ) ) ;
#4461 = CARTESIAN_POINT ( 'NONE',  ( 2.009434425284166714, 29.05181478867270783, -0.7974684545092869392 ) ) ;
#4462 = EDGE_CURVE ( 'NONE', #2681, #19197, #19467, .T. ) ;
#4463 = CARTESIAN_POINT ( 'NONE',  ( -19.44985663072000293, -9.321637154864999886, 5.906755658224999372 ) ) ;
#4464 = CYLINDRICAL_SURFACE ( 'NONE', #7296, 1.750000000000000000 ) ;
#4465 = ORIENTED_EDGE ( 'NONE', *, *, #3936, .T. ) ;
#4466 = CARTESIAN_POINT ( 'NONE',  ( 12.00000000000000000, -9.392874664203999302, -3.575135015595999999 ) ) ;
#4467 = CARTESIAN_POINT ( 'NONE',  ( -4.623015465243438982, 12.49838439281774605, 1.255993161249728152 ) ) ;
#4468 = CARTESIAN_POINT ( 'NONE',  ( -3.119235558199998870, 14.27943171969000424, 5.298223175322998024 ) ) ;
#4469 = LINE ( 'NONE', #6035, #16884 ) ;
#4470 = DIRECTION ( 'NONE',  ( 1.000000000000000000, 0.000000000000000000, 0.000000000000000000 ) ) ;
#4471 = CARTESIAN_POINT ( 'NONE',  ( -15.43323841317000067, -10.79835415318000003, -0.2870680789784999520 ) ) ;
#4472 = VECTOR ( 'NONE', #3168, 1000.000000000000000 ) ;
#4473 = CARTESIAN_POINT ( 'NONE',  ( 11.50200125730999900, -7.192471199227000511, -5.535041905695000430 ) ) ;
#4474 = CARTESIAN_POINT ( 'NONE',  ( 18.93770726999534304, 2.186149537270711818, 10.20320327474726518 ) ) ;
#4475 = EDGE_CURVE ( 'NONE', #17483, #12075, #18852, .T. ) ;
#4476 = VERTEX_POINT ( 'NONE', #13755 ) ;
#4477 = CARTESIAN_POINT ( 'NONE',  ( 21.15333103379665758, 7.368134783748077510, -5.662595685174294680 ) ) ;
#4478 =( LENGTH_UNIT ( ) NAMED_UNIT ( * ) SI_UNIT ( .MILLI., .METRE. ) );
#4479 = CARTESIAN_POINT ( 'NONE',  ( 2.083590786046000343, 25.28552202384999958, 1.742323173877000198 ) ) ;
#4480 = CARTESIAN_POINT ( 'NONE',  ( 1.677186332128803858, 13.82756761789674016, -5.893844231589445037 ) ) ;
#4481 = ORIENTED_EDGE ( 'NONE', *, *, #4685, .F. ) ;
#4482 = CARTESIAN_POINT ( 'NONE',  ( -3.762852402474997859, 13.17351449657999751, -6.004728637638001132 ) ) ;
#4483 = CARTESIAN_POINT ( 'NONE',  ( -24.33938584177417397, 12.23286334202277814, -3.811912743503483636 ) ) ;
#4484 = CARTESIAN_POINT ( 'NONE',  ( -2.000000000000000000, 18.89999999999999858, 0.000000000000000000 ) ) ;
#4485 = CARTESIAN_POINT ( 'NONE',  ( 11.92450592358672345, -4.711271677206839037, 12.50004466715123819 ) ) ;
#4486 = CARTESIAN_POINT ( 'NONE',  ( 18.57372678207664407, 7.390588772882653146, 7.422355515149504868 ) ) ;
#4487 = CARTESIAN_POINT ( 'NONE',  ( -4.473272619823412732, 13.51709772982548863, 5.071849929001408519 ) ) ;
#4488 = DIRECTION ( 'NONE',  ( 0.000000000000000000, 0.000000000000000000, -1.000000000000000000 ) ) ;
#4489 = EDGE_CURVE ( 'NONE', #903, #10311, #9568, .T. ) ;
#4490 = ORIENTED_EDGE ( 'NONE', *, *, #3324, .F. ) ;
#4491 = CARTESIAN_POINT ( 'NONE',  ( 19.07919363423065207, -2.897106654752859889, 10.08163500782726452 ) ) ;
#4492 = AXIS2_PLACEMENT_3D ( 'NONE', #20335, #3521, #16450 ) ;
#4493 = CARTESIAN_POINT ( 'NONE',  ( 11.39490977864459254, -9.382231423108610358, 8.749413452969770688 ) ) ;
#4494 = ORIENTED_EDGE ( 'NONE', *, *, #16073, .T. ) ;
#4495 = CARTESIAN_POINT ( 'NONE',  ( -1.401027947687027320, 24.49235475105247772, -1.687018025696104040 ) ) ;
#4496 = CARTESIAN_POINT ( 'NONE',  ( -0.9083185118202660169, 12.83142204585589141, 6.609727340865822143 ) ) ;
#4497 = B_SPLINE_CURVE_WITH_KNOTS ( 'NONE', 3,
 ( #18899, #18772, #6178, #9576, #2308, #21074, #16961, #4486, #17077, #6296, #474, #15245, #2542, #22637, #6049, #4253, #11876, #19010, #11757, #2423, #9812, #17197, #592, #22415, #7995, #22759, #13678, #13565, #9932, #19129, #17318, #7642, #721, #10063, #15494, #239, #13205, #15015, #8490, #15610, #3044, #13800, #19387, #8244, #12370, #15856, #21199, #12124, #23363, #841, #6781, #10181, #12247, #10302, #14052, #6905, #14173, #4983, #5103, #12003, #10550, #23245, #10431, #964, #17821, #8731, #6658, #13928, #17571, #19758, #21323, #1092, #1216, #8607, #3167, #21572, #15731, #16092, #8363, #14298, #4614, #17693, #19869, #4738, #2921, #21445, #2799, #23118, #22998, #17934, #23493, #21691, #6544, #19511, #4859, #12484, #3285, #17448, #5447, #3628, #9314, #23839, #1585, #18288, #22255, #1688, #16688, #14410, #7133, #18516, #21802 ),
 .UNSPECIFIED., .F., .F.,
 ( 4, 2, 2, 2, 1, 2, 2, 2, 2, 2, 2, 2, 2, 2, 2, 2, 2, 2, 2, 2, 2, 2, 2, 2, 2, 2, 1, 2, 2, 2, 2, 2, 2, 2, 2, 2, 2, 2, 2, 2, 2, 2, 2, 2, 2, 2, 2, 2, 2, 2, 1, 2, 2, 2, 2, 2, 4 ),
 ( 0.000000000000000000, 0.01562500000000002429, 0.03125000000000004857, 0.04687500000000006939, 0.06250000000000009714, 0.07812500000000012490, 0.09375000000000012490, 0.1093750000000001388, 0.1250000000000001388, 0.1406250000000001665, 0.1562500000000001943, 0.1718750000000001943, 0.1875000000000001665, 0.2187500000000001665, 0.2500000000000001665, 0.2812500000000001665, 0.3125000000000001665, 0.3281250000000001665, 0.3437500000000001665, 0.3593750000000001110, 0.3750000000000000555, 0.3906250000000000555, 0.4062500000000000000, 0.4218750000000000000, 0.4374999999999999445, 0.4531249999999999445, 0.4687499999999998890, 0.4843749999999998890, 0.4999999999999998335, 0.5156249999999997780, 0.5312499999999997780, 0.5468749999999998890, 0.5624999999999998890, 0.5781249999999998890, 0.5937499999999998890, 0.6093750000000000000, 0.6250000000000000000, 0.6562499999999998890, 0.6874999999999998890, 0.7187499999999997780, 0.7499999999999996669, 0.7656249999999997780, 0.7812499999999997780, 0.7968749999999997780, 0.8124999999999997780, 0.8281249999999998890, 0.8437499999999998890, 0.8593749999999998890, 0.8749999999999998890, 0.8906249999999998890, 0.9062500000000000000, 0.9218750000000000000, 0.9375000000000000000, 0.9531250000000000000, 0.9687500000000001110, 0.9843750000000001110, 1.000000000000000000 ),
 .UNSPECIFIED. ) ;
#4498 = DIRECTION ( 'NONE',  ( 0.000000000000000000, 0.000000000000000000, -1.000000000000000000 ) ) ;
#4499 = CARTESIAN_POINT ( 'NONE',  ( -21.02465558280167102, 9.210815812710263728, 1.074409851512047709 ) ) ;
#4500 = EDGE_CURVE ( 'NONE', #18008, #2459, #16907, .T. ) ;
#4501 = LINE ( 'NONE', #15623, #14422 ) ;
#4502 = ORIENTED_EDGE ( 'NONE', *, *, #2004, .T. ) ;
#4503 = ORIENTED_EDGE ( 'NONE', *, *, #15315, .F. ) ;
#4504 = CARTESIAN_POINT ( 'NONE',  ( -14.00000000000000178, 6.538808555185156024, -6.342236805579152481 ) ) ;
#4505 = CARTESIAN_POINT ( 'NONE',  ( 2.649379677055639259, 24.52555747447238588, 3.089210087447479491 ) ) ;
#4506 = PLANE ( 'NONE',  #9800 ) ;
#4507 = EDGE_CURVE ( 'NONE', #3740, #11779, #23881, .T. ) ;
#4508 = ORIENTED_EDGE ( 'NONE', *, *, #17535, .T. ) ;
#4509 = EDGE_CURVE ( 'NONE', #5868, #7294, #13430, .T. ) ;
#4510 = CARTESIAN_POINT ( 'NONE',  ( 3.099999999996331468, 15.00000000000000000, 5.570939913765761767E-07 ) ) ;
#4511 = AXIS2_PLACEMENT_3D ( 'NONE', #18991, #13657, #8108 ) ;
#4512 = LINE ( 'NONE', #11903, #993 ) ;
#4513 = CARTESIAN_POINT ( 'NONE',  ( 15.67109199796810870, -8.941468266330055314, 5.214144890658016784 ) ) ;
#4514 = VECTOR ( 'NONE', #531, 1000.000000000000114 ) ;
#4515 = CARTESIAN_POINT ( 'NONE',  ( -14.73144114140000127, 5.129804779319999675, 9.743316905584000764 ) ) ;
#4516 = CARTESIAN_POINT ( 'NONE',  ( 0.3502059142680099546, 24.70197603011302334, 4.416610674642952539 ) ) ;
#4517 = CARTESIAN_POINT ( 'NONE',  ( -20.66446177431374664, 5.378666414508218807, -9.027109991765231101 ) ) ;
#4518 = DIRECTION ( 'NONE',  ( 1.000000000000000000, 0.000000000000000000, 0.000000000000000000 ) ) ;
#4519 = CARTESIAN_POINT ( 'NONE',  ( -1.819570094927574155, 29.47616403948960695, 1.164058689780290035 ) ) ;
#4520 = EDGE_CURVE ( 'NONE', #3424, #6263, #19167, .T. ) ;
#4521 = ORIENTED_EDGE ( 'NONE', *, *, #15001, .F. ) ;
#4522 = CIRCLE ( 'NONE', #21151, 4.000000000000000000 ) ;
#4523 = CARTESIAN_POINT ( 'NONE',  ( 0.5161842332063000249, 23.85017497135000042, 2.291468635377000407 ) ) ;
#4524 = CARTESIAN_POINT ( 'NONE',  ( -15.90997336282494068, -10.10479736080180935, 2.829305410829486167 ) ) ;
#4525 = VECTOR ( 'NONE', #4201, 1000.000000000000000 ) ;
#4526 = ORIENTED_EDGE ( 'NONE', *, *, #16296, .F. ) ;
#4527 = CARTESIAN_POINT ( 'NONE',  ( 6.081233116141000927, 14.07697478751998865, -0.1743049402906998169 ) ) ;
#4528 = CARTESIAN_POINT ( 'NONE',  ( 12.00000000000000000, -8.391897884961000642, -3.194141202603999918 ) ) ;
#4529 = AXIS2_PLACEMENT_3D ( 'NONE', #12413, #1506, #14216 ) ;
#4530 = CARTESIAN_POINT ( 'NONE',  ( -24.50000000000000000, 2.477372277342497320, -10.08213454178133262 ) ) ;
#4531 = CARTESIAN_POINT ( 'NONE',  ( 18.68456408531000079, -2.737678269967000144, 9.911560247287001246 ) ) ;
#4532 = ORIENTED_EDGE ( 'NONE', *, *, #20755, .T. ) ;
#4533 = CARTESIAN_POINT ( 'NONE',  ( -20.25016455292000117, -8.657612072530000091, 3.085311466348000131 ) ) ;
#4534 = SPHERICAL_SURFACE ( 'NONE', #9177, 12.50000000000000000 ) ;
#4535 = DIRECTION ( 'NONE',  ( 0.000000000000000000, 0.000000000000000000, -1.000000000000000000 ) ) ;
#4536 = VERTEX_POINT ( 'NONE', #10137 ) ;
#4537 = CARTESIAN_POINT ( 'NONE',  ( 4.000000000000000000, 26.41693820796410108, -1.184172465503444904 ) ) ;
#4538 = CARTESIAN_POINT ( 'NONE',  ( 21.88941666666665853, -8.992648239743624927, 2.416837407849719899 ) ) ;
#4539 = CARTESIAN_POINT ( 'NONE',  ( -7.500000000000000000, -10.00000000000000000, 0.000000000000000000 ) ) ;
#4540 = DIRECTION ( 'NONE',  ( -1.000000000000000000, 0.000000000000000000, -1.562512024529000220E-11 ) ) ;
#4541 = CARTESIAN_POINT ( 'NONE',  ( 18.24479701682594524, 5.317422275654474007, -8.971661253277336101 ) ) ;
#4542 = AXIS2_PLACEMENT_3D ( 'NONE', #3723, #23945, #14963 ) ;
#4543 = CARTESIAN_POINT ( 'NONE',  ( -19.24432910583999856, 9.165129126472001175, 0.000000000000000000 ) ) ;
#4544 = CARTESIAN_POINT ( 'NONE',  ( -14.47793699669620082, -9.918738539658672693, 7.820229401576953343 ) ) ;
#4545 = CARTESIAN_POINT ( 'NONE',  ( 21.00559437492999848, -10.99239965671000085, -2.243720458468000167 ) ) ;
#4546 = AXIS2_PLACEMENT_3D ( 'NONE', #10652, #7233, #21902 ) ;
#4547 = CARTESIAN_POINT ( 'NONE',  ( 2.273493636278927976, 26.37349363267965074, -0.1540032442819480318 ) ) ;
#4548 = CARTESIAN_POINT ( 'NONE',  ( -3.814110361793421777, 14.06619296737819091, -4.853167711928797701 ) ) ;
#4549 = DIRECTION ( 'NONE',  ( 0.000000000000000000, 1.000000000000000000, 0.000000000000000000 ) ) ;
#4550 = AXIS2_PLACEMENT_3D ( 'NONE', #6128, #432, #20917 ) ;
#4551 = CARTESIAN_POINT ( 'NONE',  ( -2.146022825185431859, 30.18926127037506646, -0.2447506456446620349 ) ) ;
#4552 = EDGE_CURVE ( 'NONE', #23163, #11582, #6373, .T. ) ;
#4553 = ORIENTED_EDGE ( 'NONE', *, *, #8381, .F. ) ;
#4554 = CARTESIAN_POINT ( 'NONE',  ( 23.11666699040146256, 6.120247413312933205, 6.979269264195818501 ) ) ;
#4555 = CARTESIAN_POINT ( 'NONE',  ( 20.27958633591999771, 5.102243454006000434, 9.587269077152999586 ) ) ;
#4556 = CARTESIAN_POINT ( 'NONE',  ( 0.4857502373169989007, 12.81005527578991021, -6.651029881555492018 ) ) ;
#4557 = CARTESIAN_POINT ( 'NONE',  ( -2.434931691670788378, 27.46753006952333109, 0.6543697108982053923 ) ) ;
#4558 = CARTESIAN_POINT ( 'NONE',  ( -20.02841779011528445, 9.302829480802380147, 4.853780416162542188 ) ) ;
#4559 = CARTESIAN_POINT ( 'NONE',  ( -24.49594166687721497, -11.08137607233546262, -5.806427241621102020 ) ) ;
#4560 = CIRCLE ( 'NONE', #3419, 3.000000000000000000 ) ;
#4561 = AXIS2_PLACEMENT_3D ( 'NONE', #21253, #9359, #7177 ) ;
#4562 = CARTESIAN_POINT ( 'NONE',  ( -2.200752960429002592, 11.65894100333001049, -4.414476351808999333 ) ) ;
#4563 = ORIENTED_EDGE ( 'NONE', *, *, #14508, .T. ) ;
#4564 = DIRECTION ( 'NONE',  ( 0.000000000000000000, 1.000000000000000000, 0.000000000000000000 ) ) ;
#4565 = CARTESIAN_POINT ( 'NONE',  ( 0.5551539414043799026, 26.26248452079970619, 2.089084675604010233 ) ) ;
#4566 = CARTESIAN_POINT ( 'NONE',  ( -0.2092130522973276729, 28.61742282545599281, 2.160054418272680632 ) ) ;
#4567 = ORIENTED_EDGE ( 'NONE', *, *, #11737, .T. ) ;
#4568 = ORIENTED_EDGE ( 'NONE', *, *, #20286, .F. ) ;
#4569 = CARTESIAN_POINT ( 'NONE',  ( -12.25000000000000000, 15.43375672974000068, 0.000000000000000000 ) ) ;
#4570 = CARTESIAN_POINT ( 'NONE',  ( 19.04006424931000296, -6.376715009848999749, 8.397789983599000863 ) ) ;
#4571 = CARTESIAN_POINT ( 'NONE',  ( -20.52603093369999954, 8.128879616565001243, -7.602789782659999496 ) ) ;
#4572 = CARTESIAN_POINT ( 'NONE',  ( -16.03545417928000205, -10.81513078882999856, -0.2875120158770000378 ) ) ;
#4573 = CARTESIAN_POINT ( 'NONE',  ( -0.1752525090037950484, 24.75094615491814665, 4.517620070267612142 ) ) ;
#4574 = CARTESIAN_POINT ( 'NONE',  ( 15.46437451745999958, 7.273707250726999973, -6.465632430407000086 ) ) ;
#4575 = CARTESIAN_POINT ( 'NONE',  ( -1.606544753322670216, 28.69849995987307523, 1.460805988974954728 ) ) ;
#4576 = AXIS2_PLACEMENT_3D ( 'NONE', #10584, #1374, #16127 ) ;
#4577 = CARTESIAN_POINT ( 'NONE',  ( -0.3272492347489284192, 26.81753006952333251, 2.500000000000001332 ) ) ;
#4578 = DIRECTION ( 'NONE',  ( 0.000000000000000000, -1.000000000000000000, 0.000000000000000000 ) ) ;
#4579 = PRODUCT_DEFINITION_SHAPE ( 'NONE', 'NONE',  #23969 ) ;
#4580 = CARTESIAN_POINT ( 'NONE',  ( 5.972633094028000578, 13.70648281483999931, -2.690721685423999698 ) ) ;
#4581 = ORIENTED_EDGE ( 'NONE', *, *, #42, .F. ) ;
#4582 = CARTESIAN_POINT ( 'NONE',  ( -2.122717293740024047, 13.91157511087565801, 5.745406846198405582 ) ) ;
#4583 = CARTESIAN_POINT ( 'NONE',  ( -0.3381971108622000011, 28.03163313894999931, 2.445091418594000032 ) ) ;
#4584 = CARTESIAN_POINT ( 'NONE',  ( 1.622513874808999113, 11.61236050540001408, 4.518257084142999425 ) ) ;
#4585 = CARTESIAN_POINT ( 'NONE',  ( 0.9799592777482039052, 28.86341118070886225, 1.932436292759031726 ) ) ;
#4586 = CIRCLE ( 'NONE', #13453, 15.43375672974000068 ) ;
#4587 = AXIS2_PLACEMENT_3D ( 'NONE', #15698, #23087, #21539 ) ;
#4588 = CARTESIAN_POINT ( 'NONE',  ( -22.91770619432000089, -5.961201402843000707, -9.398931195371998726 ) ) ;
#4589 = PLANE ( 'NONE',  #13873 ) ;
#4590 = AXIS2_PLACEMENT_3D ( 'NONE', #19971, #14510, #21903 ) ;
#4591 = ORIENTED_EDGE ( 'NONE', *, *, #21054, .F. ) ;
#4592 = ADVANCED_FACE ( 'NONE', ( #6503 ), #4699, .F. ) ;
#4593 = CARTESIAN_POINT ( 'NONE',  ( -24.27585716845587172, 3.329860787255026988, -12.49993117326402725 ) ) ;
#4594 = DIRECTION ( 'NONE',  ( 0.5000000000000172085, -0.8660254037844288266, 0.000000000000000000 ) ) ;
#4595 = CARTESIAN_POINT ( 'NONE',  ( 2.226738457365001533, 12.92672802123999354, 6.099565130748998421 ) ) ;
#4596 = AXIS2_PLACEMENT_3D ( 'NONE', #3446, #21842, #5255 ) ;
#4597 = CARTESIAN_POINT ( 'NONE',  ( -1.750000000000000000, 7.000000000000000000, 0.000000000000000000 ) ) ;
#4598 = DIRECTION ( 'NONE',  ( 0.000000000000000000, -1.000000000000000000, 0.000000000000000000 ) ) ;
#4599 = CARTESIAN_POINT ( 'NONE',  ( 1.999167105995449445, 27.11753006952333322, -1.536366799937288530 ) ) ;
#4600 = CARTESIAN_POINT ( 'NONE',  ( -18.31782136596999777, 10.89202446812999980, 3.425794516969999925 ) ) ;
#4601 = CARTESIAN_POINT ( 'NONE',  ( 12.37950125730999851, 7.739157895793999487, 4.784640364371000487 ) ) ;
#4602 = CARTESIAN_POINT ( 'NONE',  ( 6.696152422707000618, 26.50000000000000000, -6.000000000000000000 ) ) ;
#4603 = CIRCLE ( 'NONE', #20848, 3.100000000000000089 ) ;
#4604 = ORIENTED_EDGE ( 'NONE', *, *, #14673, .F. ) ;
#4605 = CARTESIAN_POINT ( 'NONE',  ( -22.60725550533547334, 5.683890395623710567, 7.397078122659952903 ) ) ;
#4606 = CARTESIAN_POINT ( 'NONE',  ( -1.031996076613000080, 31.00953293605000027, -2.230181950283000258 ) ) ;
#4607 = DIRECTION ( 'NONE',  ( -0.000000000000000000, 1.000000000000000000, -0.000000000000000000 ) ) ;
#4608 = CARTESIAN_POINT ( 'NONE',  ( 1.115062346912461422, 13.75187981430681994, -6.022941901177309099 ) ) ;
#4609 = AXIS2_PLACEMENT_3D ( 'NONE', #18480, #16537, #1893 ) ;
#4610 = CARTESIAN_POINT ( 'NONE',  ( 3.471681479329000730, 13.09611127607998604, -6.183014710993997021 ) ) ;
#4611 = LINE ( 'NONE', #2418, #7693 ) ;
#4612 = CARTESIAN_POINT ( 'NONE',  ( -6.250000000000000000, 1.301187224093999891E-14, 0.000000000000000000 ) ) ;
#4613 = DIRECTION ( 'NONE',  ( 0.000000000000000000, -1.000000000000000000, 0.000000000000000000 ) ) ;
#4614 = CARTESIAN_POINT ( 'NONE',  ( 14.78242786698757527, 10.12212803168152320, 2.276770427703745714 ) ) ;
#4615 = CARTESIAN_POINT ( 'NONE',  ( -9.042815982636001948, 20.50000000000000000, 1.000000000000000000 ) ) ;
#4616 = CARTESIAN_POINT ( 'NONE',  ( -6.250000000003000267, 15.09565008225999883, -3.212814891752000079 ) ) ;
#4617 = CARTESIAN_POINT ( 'NONE',  ( -24.50000000000293454, -10.69708164072830847, 6.472111105557278421 ) ) ;
#4618 = ORIENTED_EDGE ( 'NONE', *, *, #2464, .T. ) ;
#4619 = CARTESIAN_POINT ( 'NONE',  ( -24.49999999999999645, -9.591485339921462128, -4.011769179669027352 ) ) ;
#4620 = CARTESIAN_POINT ( 'NONE',  ( -1.256379856539187267, 11.63154580748610911, -4.622687534862957470 ) ) ;
#4621 = VERTEX_POINT ( 'NONE', #7957 ) ;
#4622 = AXIS2_PLACEMENT_3D ( 'NONE', #13448, #6057, #20850 ) ;
#4623 = EDGE_CURVE ( 'NONE', #16623, #2832, #21501, .T. ) ;
#4624 = CARTESIAN_POINT ( 'NONE',  ( 0.7194182799258999061, 25.89386557969000080, 2.640899101350000056 ) ) ;
#4625 = CARTESIAN_POINT ( 'NONE',  ( -0.3561344694547327050, 24.42488000727052011, -2.163805914283786880 ) ) ;
#4626 = CARTESIAN_POINT ( 'NONE',  ( -4.254430764150507471, 13.40513193608355103, 5.356630145924516917 ) ) ;
#4627 = VECTOR ( 'NONE', #21697, 1000.000000000000227 ) ;
#4628 = CARTESIAN_POINT ( 'NONE',  ( 16.75703476075999987, 10.47950889854999801, -3.590276921464000015 ) ) ;
#4629 = CARTESIAN_POINT ( 'NONE',  ( -5.330032540885996539, 15.50909013537999037, -2.864334533482998602 ) ) ;
#4630 = AXIS2_PLACEMENT_3D ( 'NONE', #8606, #8730, #4613 ) ;
#4631 = CARTESIAN_POINT ( 'NONE',  ( 2.747163055864000114, 25.41169433610000183, -0.8328668639933000106 ) ) ;
#4632 = EDGE_LOOP ( 'NONE', ( #10454, #8516 ) ) ;
#4633 = ORIENTED_EDGE ( 'NONE', *, *, #20520, .F. ) ;
#4634 = CARTESIAN_POINT ( 'NONE',  ( -14.00000000000000355, -9.419675942593046969, -3.728492687917730031 ) ) ;
#4635 = CARTESIAN_POINT ( 'NONE',  ( -1.419111322447411450, 6.922937340745385804, -1.049103944711770708 ) ) ;
#4636 = FACE_OUTER_BOUND ( 'NONE', #16977, .T. ) ;
#4637 = ORIENTED_EDGE ( 'NONE', *, *, #16712, .F. ) ;
#4638 = EDGE_CURVE ( 'NONE', #12888, #2273, #980, .T. ) ;
#4639 = DIRECTION ( 'NONE',  ( -1.000000000000000000, 0.000000000000000000, 0.000000000000000000 ) ) ;
#4640 = CARTESIAN_POINT ( 'NONE',  ( -2.000000000000000000, 28.00000000000000000, -3.464101615137999968 ) ) ;
#4641 = CARTESIAN_POINT ( 'NONE',  ( 15.15874227237765659, 6.918783474670889611, 7.681163286608844842 ) ) ;
#4642 = CARTESIAN_POINT ( 'NONE',  ( -16.39145269483999812, 4.899706566793000206, 9.911772188210001389 ) ) ;
#4643 = CONICAL_SURFACE ( 'NONE', #14307, 2.849999992212000066, 0.7853981633972997312 ) ;
#4644 = LINE ( 'NONE', #6203, #14553 ) ;
#4645 = CARTESIAN_POINT ( 'NONE',  ( -20.02108363062186669, 3.882350337173073207, 9.834850751737567620 ) ) ;
#4646 = CARTESIAN_POINT ( 'NONE',  ( 4.736747859573000596, 12.61325828439998986, 0.1514365790727000005 ) ) ;
#4647 = CARTESIAN_POINT ( 'NONE',  ( -16.28651788626999775, 5.579994563924000062, 9.896790535726999849 ) ) ;
#4648 = EDGE_CURVE ( 'NONE', #19046, #11301, #372, .T. ) ;
#4649 = CARTESIAN_POINT ( 'NONE',  ( -1.913666731007989785, 29.46549386981544316, 1.007641490493420777 ) ) ;
#4650 = ORIENTED_EDGE ( 'NONE', *, *, #20761, .T. ) ;
#4651 = CARTESIAN_POINT ( 'NONE',  ( -1.347470520100000124, 25.07321246089999889, -1.721172773618999896 ) ) ;
#4652 = CARTESIAN_POINT ( 'NONE',  ( -16.02573005821852092, -8.129144771390043545, 6.492559992316535578 ) ) ;
#4653 = CONICAL_SURFACE ( 'NONE', #18200, 3.049999825846000157, 0.7853981633972997312 ) ;
#4654 = VERTEX_POINT ( 'NONE', #12202 ) ;
#4655 = EDGE_CURVE ( 'NONE', #18177, #23789, #8686, .T. ) ;
#4656 = CARTESIAN_POINT ( 'NONE',  ( 5.190852480600997687, 14.34138478008000206, -3.176459389033000846 ) ) ;
#4657 = CARTESIAN_POINT ( 'NONE',  ( 12.00000000000000000, -6.617649098573062716, -6.069521219509731225 ) ) ;
#4658 = CARTESIAN_POINT ( 'NONE',  ( 17.46779166666665617, 9.119539674411541341, 1.193618004230074803 ) ) ;
#4659 = B_SPLINE_CURVE_WITH_KNOTS ( 'NONE', 3,
 ( #11216, #9036, #7558, #18245, #16530, #18354, #18704, #14712, #10969, #2112, #22104, #7205, #12892, #9503, #14936, #16647, #11333, #22332, #5747, #16877, #284, #9385, #13010, #5406, #3819, #14483, #5628, #20292, #16406 ),
 .UNSPECIFIED., .F., .F.,
 ( 4, 2, 1, 1, 1, 2, 2, 2, 1, 1, 1, 2, 2, 2, 1, 2, 2, 4 ),
 ( 0.000000000000000000, 0.1249999999999825695, 0.1874999999999737987, 0.2187499999999698852, 0.2343749999999678313, 0.2421874999999675537, 0.2499999999999673039, 0.3749999999999690803, 0.4374999999999704126, 0.4687499999999713562, 0.4843749999999720779, 0.4921874999999727440, 0.4999999999999733546, 0.6249999999999801270, 0.6874999999999827915, 0.7187499999999846789, 0.7499999999999865663, 1.000000000000000000 ),
 .UNSPECIFIED. ) ;
#4660 = CARTESIAN_POINT ( 'NONE',  ( 13.50281392131000047, -8.671483154093998280, -4.205333541112000084 ) ) ;
#4661 = VERTEX_POINT ( 'NONE', #17776 ) ;
#4662 = B_SPLINE_CURVE_WITH_KNOTS ( 'NONE', 3,
 ( #8245, #11878, #17449, #15734, #19130 ),
 .UNSPECIFIED., .F., .F.,
 ( 4, 1, 4 ),
 ( 0.000000000000000000, 0.5000000000000000000, 1.000000000000000000 ),
 .UNSPECIFIED. ) ;
#4663 = CARTESIAN_POINT ( 'NONE',  ( -11.94558899291999943, 2.716703440716999651, -13.81957412132000051 ) ) ;
#4664 = CARTESIAN_POINT ( 'NONE',  ( 2.500000000000000000, 26.81666666666667354, -0.3272492347489370235 ) ) ;
#4665 = FACE_OUTER_BOUND ( 'NONE', #8234, .T. ) ;
#4666 = VERTEX_POINT ( 'NONE', #6737 ) ;
#4667 = EDGE_CURVE ( 'NONE', #1513, #1991, #3243, .T. ) ;
#4668 = FACE_OUTER_BOUND ( 'NONE', #6237, .T. ) ;
#4669 = CARTESIAN_POINT ( 'NONE',  ( 12.40357033521693175, 7.855338663088507367, 11.39415432486939572 ) ) ;
#4670 = CARTESIAN_POINT ( 'NONE',  ( 1.709999999999999964, 9.852710287022999225, 7.500000000000000000 ) ) ;
#4671 = CARTESIAN_POINT ( 'NONE',  ( -14.00000000000000000, -4.764382124690100362, 8.836888828107323235 ) ) ;
#4672 = CARTESIAN_POINT ( 'NONE',  ( 17.46750683744905785, -8.705786543820593693, 5.763209729995592667 ) ) ;
#4673 = FACE_OUTER_BOUND ( 'NONE', #19178, .T. ) ;
#4674 = CARTESIAN_POINT ( 'NONE',  ( -14.44600769525627726, 12.24671445775786971, -3.788037462221122809 ) ) ;
#4675 = CARTESIAN_POINT ( 'NONE',  ( 21.37268830086000193, -1.097984307014999938, -11.17531938858999929 ) ) ;
#4676 = CARTESIAN_POINT ( 'NONE',  ( -8.250000000000000000, 23.50000000000000000, 1.000000000000000000 ) ) ;
#4677 = DIRECTION ( 'NONE',  ( 1.000000000000000000, 0.000000000000000000, 0.000000000000000000 ) ) ;
#4678 = CARTESIAN_POINT ( 'NONE',  ( 12.50897833293000083, 7.466860214713999966, -11.77832264250999827 ) ) ;
#4679 = CARTESIAN_POINT ( 'NONE',  ( -2.144040404256133847, 30.18827354168691812, -0.2615996283942206291 ) ) ;
#4680 = ORIENTED_EDGE ( 'NONE', *, *, #21353, .F. ) ;
#4681 = CARTESIAN_POINT ( 'NONE',  ( 22.90890952007856995, 9.256333691698992894, 1.211909054350287507 ) ) ;
#4682 = CARTESIAN_POINT ( 'NONE',  ( 24.72435780780000059, -7.322751853928000543, -7.090892171531000265 ) ) ;
#4683 = CARTESIAN_POINT ( 'NONE',  ( 4.000000000000000000, 28.30000000000000071, -2.309401076759000304 ) ) ;
#4684 = CARTESIAN_POINT ( 'NONE',  ( -1.976671150083846973, 23.62257745056772862, -0.7977860612064010537 ) ) ;
#4685 = EDGE_CURVE ( 'NONE', #4621, #19823, #3000, .T. ) ;
#4686 = CARTESIAN_POINT ( 'NONE',  ( 0.2604860018441254588, 24.64510472144360165, 2.238162498141799794 ) ) ;
#4687 = CARTESIAN_POINT ( 'NONE',  ( 4.843572631659477601, 14.61404048541572820, 3.775228271240138156 ) ) ;
#4688 = EDGE_CURVE ( 'NONE', #13175, #16279, #18015, .T. ) ;
#4689 = CARTESIAN_POINT ( 'NONE',  ( -2.202567442112000062, 11.73255007762998581, -4.445896772107005290 ) ) ;
#4690 = ORIENTED_EDGE ( 'NONE', *, *, #2225, .F. ) ;
#4691 = CARTESIAN_POINT ( 'NONE',  ( -14.69785853588606450, 10.31120977210299117, 0.9820122563291259210 ) ) ;
#4692 = CARTESIAN_POINT ( 'NONE',  ( -4.000000000000000000, 29.69999999999999929, -2.309401076759000304 ) ) ;
#4693 = DIRECTION ( 'NONE',  ( -0.000000000000000000, 1.000000000000000000, -0.000000000000000000 ) ) ;
#4694 = CONICAL_SURFACE ( 'NONE', #3906, 9.161549281532000322, 0.02565634000431304615 ) ;
#4695 = CARTESIAN_POINT ( 'NONE',  ( 0.000000000000000000, 0.000000000000000000, 0.000000000000000000 ) ) ;
#4696 = DIRECTION ( 'NONE',  ( -1.000000000000000000, 0.000000000000000000, 0.000000000000000000 ) ) ;
#4697 = ORIENTED_EDGE ( 'NONE', *, *, #3215, .F. ) ;
#4698 = EDGE_CURVE ( 'NONE', #1429, #23795, #19020, .T. ) ;
#4699 = PLANE ( 'NONE',  #15749 ) ;
#4700 = EDGE_CURVE ( 'NONE', #44, #11336, #12559, .T. ) ;
#4701 = CARTESIAN_POINT ( 'NONE',  ( -12.47890960666999938, 9.613013645102999050, -12.04164784824000023 ) ) ;
#4702 = CARTESIAN_POINT ( 'NONE',  ( -23.36459867855000283, -10.41392035115000070, 2.403458430719999761 ) ) ;
#4703 = CARTESIAN_POINT ( 'NONE',  ( -14.07020113697999975, -0.8985174727690999896, -10.18952336305999928 ) ) ;
#4704 = CARTESIAN_POINT ( 'NONE',  ( -6.222637507652000188, 15.85814527750000913, 1.061553398158999517 ) ) ;
#4705 = CARTESIAN_POINT ( 'NONE',  ( 19.12062451746000136, 7.953000653253999630, -5.784009966395999847 ) ) ;
#4706 = CARTESIAN_POINT ( 'NONE',  ( -3.999999999999998224, 26.44682129341587640, -0.9440428258622635127 ) ) ;
#4707 = B_SPLINE_CURVE_WITH_KNOTS ( 'NONE', 3,
 ( #11297, #22771, #13450, #11531 ),
 .UNSPECIFIED., .F., .F.,
 ( 4, 4 ),
 ( 0.6207796204815331231, 1.000000000000000000 ),
 .UNSPECIFIED. ) ;
#4708 = DIRECTION ( 'NONE',  ( 1.000000000000000000, 0.000000000000000000, 0.000000000000000000 ) ) ;
#4709 = CARTESIAN_POINT ( 'NONE',  ( 0.000000000000000000, 24.65000000000000213, 0.000000000000000000 ) ) ;
#4710 = VERTEX_POINT ( 'NONE', #4938 ) ;
#4711 = CARTESIAN_POINT ( 'NONE',  ( 0.6113494706473727724, 13.70697912404423491, 6.098629219130683232 ) ) ;
#4712 = CARTESIAN_POINT ( 'NONE',  ( -0.8137643771028287842, 24.74949622857204901, 2.006896345404644233 ) ) ;
#4713 = DIRECTION ( 'NONE',  ( 1.000000000000000000, 0.000000000000000000, 0.000000000000000000 ) ) ;
#4714 = CARTESIAN_POINT ( 'NONE',  ( -20.07726891605999953, 1.668335638170999946, 10.92619773972000097 ) ) ;
#4715 = DIRECTION ( 'NONE',  ( 0.000000000000000000, 1.000000000000000000, 0.000000000000000000 ) ) ;
#4716 = ORIENTED_EDGE ( 'NONE', *, *, #7876, .T. ) ;
#4717 = CARTESIAN_POINT ( 'NONE',  ( -23.74465998031000069, -13.93375672974000068, 0.8660254037843999608 ) ) ;
#4718 = CARTESIAN_POINT ( 'NONE',  ( 4.262829215123017157, 12.23638733703982773, -2.301400808804427101 ) ) ;
#4719 = CARTESIAN_POINT ( 'NONE',  ( -3.887848091610002221, 14.54074437727999225, 4.743303306622997262 ) ) ;
#4720 = CARTESIAN_POINT ( 'NONE',  ( -0.9439381825837785955, 6.842295547824369883, 1.479774886885111274 ) ) ;
#4721 = CARTESIAN_POINT ( 'NONE',  ( 0.000000000000000000, 22.00000000000000000, 0.000000000000000000 ) ) ;
#4722 = CYLINDRICAL_SURFACE ( 'NONE', #14841, 2.500000000000000000 ) ;
#4723 = CARTESIAN_POINT ( 'NONE',  ( -19.46889333780000086, -9.261490887677000572, 5.613638565637999456 ) ) ;
#4724 = CARTESIAN_POINT ( 'NONE',  ( 13.36668875730999950, -6.148145076040000490, -6.742444596879999530 ) ) ;
#4725 = CARTESIAN_POINT ( 'NONE',  ( 18.96142490315194706, 1.354195692915298732, 10.35531029028993011 ) ) ;
#4726 = CONICAL_SURFACE ( 'NONE', #5867, 14.37500000000000000, 0.7853981633972997312 ) ;
#4727 = ORIENTED_EDGE ( 'NONE', *, *, #3293, .T. ) ;
#4728 = CARTESIAN_POINT ( 'NONE',  ( -6.042815982636000172, 21.50000000000000000, 1.000000000000000000 ) ) ;
#4729 = CARTESIAN_POINT ( 'NONE',  ( 0.5028989451434000557, 28.98002150817000100, 2.482341192449999845 ) ) ;
#4730 = B_SPLINE_CURVE_WITH_KNOTS ( 'NONE', 3,
 ( #14940, #7333, #2116, #5751, #22336, #20534, #290, #22109, #15065, #5519 ),
 .UNSPECIFIED., .F., .F.,
 ( 4, 2, 2, 2, 4 ),
 ( 0.5908772401967050669, 0.6931579301475288002, 0.7954386200983525335, 0.8977193100491762667, 1.000000000000000000 ),
 .UNSPECIFIED. ) ;
#4731 = CARTESIAN_POINT ( 'NONE',  ( -2.629981577853999664, 23.38563562995999945, 0.2328718829719999828 ) ) ;
#4732 = CARTESIAN_POINT ( 'NONE',  ( 1.048474406570862216, 13.74492151073522805, -6.034635998210232444 ) ) ;
#4733 = ORIENTED_EDGE ( 'NONE', *, *, #9700, .F. ) ;
#4734 = DIRECTION ( 'NONE',  ( 1.000000000000000000, 0.000000000000000000, 0.000000000000000000 ) ) ;
#4735 = DIRECTION ( 'NONE',  ( 0.000000000000000000, -1.000000000000000000, 0.000000000000000000 ) ) ;
#4736 = CARTESIAN_POINT ( 'NONE',  ( -1.018158653951999781, 29.62256419343999880, -2.549909324983000047 ) ) ;
#4737 = LINE ( 'NONE', #3043, #15047 ) ;
#4738 = CARTESIAN_POINT ( 'NONE',  ( 14.64304187746229502, 10.02171780537468138, -2.677710796655983660 ) ) ;
#4739 = FACE_OUTER_BOUND ( 'NONE', #14733, .T. ) ;
#4740 = CIRCLE ( 'NONE', #12085, 3.100000000000000089 ) ;
#4741 = CARTESIAN_POINT ( 'NONE',  ( 0.000000000000000000, 20.00000000000000000, -3.100000000000386002 ) ) ;
#4742 = CARTESIAN_POINT ( 'NONE',  ( -24.50000000000000000, -10.82531754731000007, 6.250000000000000000 ) ) ;
#4743 = ORIENTED_EDGE ( 'NONE', *, *, #22654, .F. ) ;
#4744 = DIRECTION ( 'NONE',  ( 0.000000000000000000, 0.7071067811866525998, -0.7071067811864425456 ) ) ;
#4745 = CARTESIAN_POINT ( 'NONE',  ( 11.48478210366629426, -9.189386602278768024, 9.083340531715208499 ) ) ;
#4746 = ORIENTED_EDGE ( 'NONE', *, *, #1055, .F. ) ;
#4747 = CARTESIAN_POINT ( 'NONE',  ( 2.600121693191999928, 24.50045998918000123, -0.8551739725367000222 ) ) ;
#4748 = DIRECTION ( 'NONE',  ( 0.000000000000000000, 1.000000000000000000, 0.000000000000000000 ) ) ;
#4749 = CARTESIAN_POINT ( 'NONE',  ( 2.656543060185477145, 13.04243739147230841, 6.182893541209614874 ) ) ;
#4750 = AXIS2_PLACEMENT_3D ( 'NONE', #11185, #16621, #384 ) ;
#4751 = CARTESIAN_POINT ( 'NONE',  ( 6.156715153800679907, 14.09036096121806736, -0.3579005024942175650 ) ) ;
#4752 = CARTESIAN_POINT ( 'NONE',  ( -20.72159387545667286, 3.650365305096916924, 8.516053178569631399 ) ) ;
#4753 = CARTESIAN_POINT ( 'NONE',  ( -1.595084814687000030, 25.89919433610000254, 2.387212940976999764 ) ) ;
#4754 = ORIENTED_EDGE ( 'NONE', *, *, #7620, .T. ) ;
#4755 = CARTESIAN_POINT ( 'NONE',  ( -4.900699999999999612, 1.284663064832999817E-14, 0.000000000000000000 ) ) ;
#4756 = CARTESIAN_POINT ( 'NONE',  ( 2.160826008357634720, 29.99999999999999645, -3.371248675920325510 ) ) ;
#4757 = DIRECTION ( 'NONE',  ( 0.000000000000000000, 0.000000000000000000, -1.000000000000000000 ) ) ;
#4758 = ORIENTED_EDGE ( 'NONE', *, *, #21648, .F. ) ;
#4759 = CARTESIAN_POINT ( 'NONE',  ( -20.60455590132000125, -6.094466645755999501, -8.781673769740001134 ) ) ;
#4760 = CARTESIAN_POINT ( 'NONE',  ( 25.72500000000000142, 0.000000000000000000, 0.000000000000000000 ) ) ;
#4761 = DIRECTION ( 'NONE',  ( 0.000000000000000000, 0.000000000000000000, -1.000000000000000000 ) ) ;
#4762 = CARTESIAN_POINT ( 'NONE',  ( 14.97329753049621637, 10.12988386828463483, 2.035425917223504744 ) ) ;
#4763 = CARTESIAN_POINT ( 'NONE',  ( -14.06900898629000096, -10.21389801573999989, -2.520607692115000020 ) ) ;
#4764 = EDGE_CURVE ( 'NONE', #20551, #5868, #20195, .T. ) ;
#4765 = CARTESIAN_POINT ( 'NONE',  ( 18.75008227645999881, 0.000000000000000000, 0.000000000000000000 ) ) ;
#4766 = CARTESIAN_POINT ( 'NONE',  ( 13.52097745565073694, 5.132826260074074831, -7.447908584389146824 ) ) ;
#4767 = CARTESIAN_POINT ( 'NONE',  ( -4.776902322660998124, 12.47834578811000483, 0.1510698533714998903 ) ) ;
#4768 = VECTOR ( 'NONE', #10319, 1000.000000000000000 ) ;
#4769 = CARTESIAN_POINT ( 'NONE',  ( -14.00000000000000000, -10.27687089286999900, -0.6428416445564000270 ) ) ;
#4770 = CARTESIAN_POINT ( 'NONE',  ( -1.854515264472811786, 29.47225744612200060, 1.107362145631518136 ) ) ;
#4771 = ORIENTED_EDGE ( 'NONE', *, *, #10719, .F. ) ;
#4772 = DIRECTION ( 'NONE',  ( 1.000000000000000000, 0.000000000000000000, 0.000000000000000000 ) ) ;
#4773 = CARTESIAN_POINT ( 'NONE',  ( -14.46301467040578892, -0.3024465970358821698, 10.35139680070230916 ) ) ;
#4774 = EDGE_LOOP ( 'NONE', ( #11243, #10368, #13428, #5434, #582, #17464 ) ) ;
#4775 = CARTESIAN_POINT ( 'NONE',  ( -23.74465998031000069, 6.216878364870000340, -12.50000000000000000 ) ) ;
#4776 = CARTESIAN_POINT ( 'NONE',  ( 4.909136497312005076, 14.89158879234001986, -3.677509687533000893 ) ) ;
#4777 = EDGE_CURVE ( 'NONE', #16006, #4621, #4160, .T. ) ;
#4778 = CARTESIAN_POINT ( 'NONE',  ( 12.00000000000000000, -5.414213694566718083, -7.209897367101869570 ) ) ;
#4779 = B_SPLINE_CURVE_WITH_KNOTS ( 'NONE', 3,
 ( #12019, #19400, #6062, #8380, #2322, #2814, #17586, #15748, #6559, #13943, #4268, #22773 ),
 .UNSPECIFIED., .F., .F.,
 ( 4, 1, 1, 1, 1, 2, 2, 4 ),
 ( 0.000000000000000000, 0.2499999999999981681, 0.3749999999999972244, 0.4374999999999967804, 0.4687499999999966138, 0.4843749999999967248, 0.4999999999999967804, 1.000000000000000000 ),
 .UNSPECIFIED. ) ;
#4780 = CARTESIAN_POINT ( 'NONE',  ( -20.37217920454666498, -8.954726317883316966, -2.406646174506601898 ) ) ;
#4781 = CARTESIAN_POINT ( 'NONE',  ( 14.29706408530999973, 7.153286345558000470, -7.225396115407999531 ) ) ;
#4782 = VERTEX_POINT ( 'NONE', #18708 ) ;
#4783 = AXIS2_PLACEMENT_3D ( 'NONE', #12261, #12387, #17949 ) ;
#4784 = CARTESIAN_POINT ( 'NONE',  ( -8.789091492920999116, 10.90342355828000009, -9.585088201729998758 ) ) ;
#4785 = DIRECTION ( 'NONE',  ( 0.000000000000000000, 0.000000000000000000, -1.000000000000000000 ) ) ;
#4786 = EDGE_LOOP ( 'NONE', ( #9976, #17842, #12505 ) ) ;
#4787 = CARTESIAN_POINT ( 'NONE',  ( 11.40904387244028939, 12.29944272054195942, 3.696645716850592400 ) ) ;
#4788 = DIRECTION ( 'NONE',  ( -1.000000000000000000, 0.000000000000000000, 0.000000000000000000 ) ) ;
#4789 = CARTESIAN_POINT ( 'NONE',  ( -4.841618408765723913, 13.27908324391153627, -5.800473559599023332 ) ) ;
#4790 = CARTESIAN_POINT ( 'NONE',  ( 16.27408216237130389, -0.09528988118115871986, -10.36544040251896526 ) ) ;
#4791 = AXIS2_PLACEMENT_3D ( 'NONE', #17101, #2562, #7900 ) ;
#4792 = DIRECTION ( 'NONE',  ( 0.000000000000000000, 0.000000000000000000, -1.000000000000000000 ) ) ;
#4793 = ADVANCED_FACE ( 'NONE', ( #16652 ), #9278, .T. ) ;
#4794 = CARTESIAN_POINT ( 'NONE',  ( -14.49863740493600339, -11.08451042427809519, 5.800992024733008456 ) ) ;
#4795 = CARTESIAN_POINT ( 'NONE',  ( -3.915804718101239423, 13.94229419359897015, -4.846387647554452727 ) ) ;
#4796 = CARTESIAN_POINT ( 'NONE',  ( -24.50000000000000000, 10.82531754731000007, -6.250000000000000000 ) ) ;
#4797 = CARTESIAN_POINT ( 'NONE',  ( -1.931946195963927915, 30.14479945992585641, -0.9657778908081225966 ) ) ;
#4798 = VERTEX_POINT ( 'NONE', #11092 ) ;
#4799 = CARTESIAN_POINT ( 'NONE',  ( -24.50000000000452971, -0.5124611670954127840, 12.50000000000233946 ) ) ;
#4800 = CARTESIAN_POINT ( 'NONE',  ( 24.14460500711999913, -3.573525003673000189, 10.36867931893000083 ) ) ;
#4801 = CARTESIAN_POINT ( 'NONE',  ( 23.50544148562050140, -1.024754352332091445, -10.55397606538692479 ) ) ;
#4802 = CARTESIAN_POINT ( 'NONE',  ( -1.999167105995446780, 27.51753006952333180, 1.536366799937292305 ) ) ;
#4803 = ORIENTED_EDGE ( 'NONE', *, *, #5527, .T. ) ;
#4804 = CARTESIAN_POINT ( 'NONE',  ( 2.151661648330430943, 24.06873469183733860, -0.6690115951027478802 ) ) ;
#4805 = FACE_OUTER_BOUND ( 'NONE', #7299, .T. ) ;
#4806 = EDGE_CURVE ( 'NONE', #15484, #18419, #18327, .T. ) ;
#4807 = CARTESIAN_POINT ( 'NONE',  ( 4.644870904606005269, 12.40269947270000372, -1.737130352826000257 ) ) ;
#4808 = ORIENTED_EDGE ( 'NONE', *, *, #11921, .T. ) ;
#4809 = CARTESIAN_POINT ( 'NONE',  ( -16.56791143023856350, 10.36026656484473563, -1.037743970940367966 ) ) ;
#4810 = CARTESIAN_POINT ( 'NONE',  ( -4.000000142211483478, 24.55137445130720053, -0.9449696197475782045 ) ) ;
#4811 = CARTESIAN_POINT ( 'NONE',  ( -1.250502274040745654, 26.95316898822477114, 1.812620555901804265 ) ) ;
#4812 = EDGE_CURVE ( 'NONE', #6384, #12389, #7691, .T. ) ;
#4813 = CARTESIAN_POINT ( 'NONE',  ( -14.41332695378262585, -3.614289100528644383, -12.49991738135552488 ) ) ;
#4814 = EDGE_LOOP ( 'NONE', ( #22596, #17054, #2284, #8840 ) ) ;
#4815 = CARTESIAN_POINT ( 'NONE',  ( -18.96831264622833757, -3.696727937718024659, 8.446581985469661547 ) ) ;
#4816 = CARTESIAN_POINT ( 'NONE',  ( -4.001664678273323617, 14.92001132474814895, -4.637136486520930134 ) ) ;
#4817 = CARTESIAN_POINT ( 'NONE',  ( -14.32510917350998803, -2.162566426017664689, -8.825035394896943330 ) ) ;
#4818 = EDGE_CURVE ( 'NONE', #18419, #23934, #3940, .T. ) ;
#4819 = CARTESIAN_POINT ( 'NONE',  ( -20.16411157606999893, -6.838742577979000536, 6.702193969124000006 ) ) ;
#4820 = CARTESIAN_POINT ( 'NONE',  ( 22.38070833333331677, -1.210375094748616709, -9.245614798928990297 ) ) ;
#4821 = EDGE_CURVE ( 'NONE', #12346, #9620, #14766, .T. ) ;
#4822 = CARTESIAN_POINT ( 'NONE',  ( 14.38056994526000132, -9.435743274165000471, 3.981841483676999527 ) ) ;
#4823 = CARTESIAN_POINT ( 'NONE',  ( -11.75044449363000076, 1.368548241523999952E-14, 0.000000000000000000 ) ) ;
#4824 = CARTESIAN_POINT ( 'NONE',  ( 19.75818759120999957, -0.05617709961787999834, 9.259200605838000087 ) ) ;
#4825 = CARTESIAN_POINT ( 'NONE',  ( 15.54041666666666011, 8.833960962437073405, -2.374191386965657458 ) ) ;
#4826 = ORIENTED_EDGE ( 'NONE', *, *, #16612, .F. ) ;
#4827 = CONICAL_SURFACE ( 'NONE', #19523, 2.249999993254999886, 0.7853981633972997312 ) ;
#4828 = LINE ( 'NONE', #8215, #16948 ) ;
#4829 = CARTESIAN_POINT ( 'NONE',  ( 1.528152797339000113, 26.76413313895000101, -1.938452583514000072 ) ) ;
#4830 = CARTESIAN_POINT ( 'NONE',  ( -20.00016243917331593, -8.025264609412063876, -4.625618550852887978 ) ) ;
#4831 = CARTESIAN_POINT ( 'NONE',  ( -23.08479074010000076, -10.13546262256000219, -4.609682220154000198 ) ) ;
#4832 = EDGE_CURVE ( 'NONE', #17213, #9887, #6170, .T. ) ;
#4833 = EDGE_CURVE ( 'NONE', #12220, #6975, #4730, .T. ) ;
#4834 = FACE_OUTER_BOUND ( 'NONE', #14080, .T. ) ;
#4835 = CIRCLE ( 'NONE', #7915, 7.500000000000000000 ) ;
#4836 = CARTESIAN_POINT ( 'NONE',  ( 0.7413504348446855463, 11.50606621628979376, 4.755316385197891904 ) ) ;
#4837 = ORIENTED_EDGE ( 'NONE', *, *, #9370, .T. ) ;
#4838 = DIRECTION ( 'NONE',  ( 0.000000000000000000, 1.000000000000000000, 0.000000000000000000 ) ) ;
#4839 = CARTESIAN_POINT ( 'NONE',  ( -24.17970357213072319, -4.108081272002119810, -12.49999456974979850 ) ) ;
#4840 = DIRECTION ( 'NONE',  ( 0.000000000000000000, 0.000000000000000000, -1.000000000000000000 ) ) ;
#4841 = MECHANICAL_DESIGN_GEOMETRIC_PRESENTATION_REPRESENTATION (  '', ( #19537 ), #22224 ) ;
#4842 = CARTESIAN_POINT ( 'NONE',  ( 11.64693288521071146, -5.045341008171505770, -7.448699753728570627 ) ) ;
#4843 = CARTESIAN_POINT ( 'NONE',  ( -3.000000000000000000, 20.00000000000000000, 0.000000000000000000 ) ) ;
#4844 = CARTESIAN_POINT ( 'NONE',  ( -1.235289751754999887, 30.50000000000000000, -2.173490103315000255 ) ) ;
#4845 = CARTESIAN_POINT ( 'NONE',  ( -16.89590893017999562, 5.628454363070000355, -9.888856528401998247 ) ) ;
#4846 = CARTESIAN_POINT ( 'NONE',  ( 12.84468892131000040, 2.447276857699999919, 9.303608529293999396 ) ) ;
#4847 = CARTESIAN_POINT ( 'NONE',  ( 18.88799200410561596, 3.848042924961065925, 9.710018918712066238 ) ) ;
#4848 = VERTEX_POINT ( 'NONE', #22459 ) ;
#4849 = CARTESIAN_POINT ( 'NONE',  ( 5.202457668997545248, 13.92662484198413786, 4.051450832662363055 ) ) ;
#4850 = CARTESIAN_POINT ( 'NONE',  ( -2.498205606922999866, 29.57563899243999828, 0.4172517292406999756 ) ) ;
#4851 = FACE_OUTER_BOUND ( 'NONE', #6824, .T. ) ;
#4852 = DIRECTION ( 'NONE',  ( 0.000000000000000000, 0.8660254037844288266, -0.5000000000000169864 ) ) ;
#4853 = AXIS2_PLACEMENT_3D ( 'NONE', #960, #6412, #13796 ) ;
#4854 = ORIENTED_EDGE ( 'NONE', *, *, #4252, .F. ) ;
#4855 = CARTESIAN_POINT ( 'NONE',  ( -0.1529142988638288181, 26.50000000000000355, -2.395123632968240823 ) ) ;
#4856 = DIRECTION ( 'NONE',  ( 0.000000000000000000, 0.000000000000000000, 1.000000000000000000 ) ) ;
#4857 = CARTESIAN_POINT ( 'NONE',  ( 12.52688711657000020, 7.716878364870000340, -11.63397459621999985 ) ) ;
#4858 = DIRECTION ( 'NONE',  ( 0.000000000000000000, -1.000000000000000000, 0.000000000000000000 ) ) ;
#4859 = CARTESIAN_POINT ( 'NONE',  ( 14.19700671098188494, -2.419028854851438481, -10.07012218490691602 ) ) ;
#4860 = FACE_OUTER_BOUND ( 'NONE', #5036, .T. ) ;
#4861 = CARTESIAN_POINT ( 'NONE',  ( -21.36066243917331420, 4.643201456420162465, -8.055771210932663351 ) ) ;
#4862 = FACE_OUTER_BOUND ( 'NONE', #4888, .T. ) ;
#4863 = EDGE_LOOP ( 'NONE', ( #5248, #105, #4224, #7535 ) ) ;
#4864 = EDGE_CURVE ( 'NONE', #13328, #15471, #23201, .T. ) ;
#4865 = CARTESIAN_POINT ( 'NONE',  ( 0.000000000000000000, 26.35000000000000142, 0.000000000000000000 ) ) ;
#4866 = CARTESIAN_POINT ( 'NONE',  ( 11.06626444616127181, -10.69977336182518890, 6.467440677471968158 ) ) ;
#4867 = VERTEX_POINT ( 'NONE', #4057 ) ;
#4868 = CARTESIAN_POINT ( 'NONE',  ( -2.694750659793999858, 24.08243831202999985, 0.4798224739857999688 ) ) ;
#4869 = CARTESIAN_POINT ( 'NONE',  ( 18.85240113949000218, -1.886779804701000041, 10.26112574610000117 ) ) ;
#4870 = CARTESIAN_POINT ( 'NONE',  ( 4.108814524948330771, 13.36799685942058424, 5.443337052582164937 ) ) ;
#4871 = TOROIDAL_SURFACE ( 'NONE', #16066, 4.649999999999999467, 0.1000000000000000056 ) ;
#4872 = CARTESIAN_POINT ( 'NONE',  ( 12.52688711657000020, 13.93375672974000068, 0.8660254037843999608 ) ) ;
#4873 = CARTESIAN_POINT ( 'NONE',  ( -1.999167105995452998, 27.91666666666667140, -1.536366799937284089 ) ) ;
#4874 = DIRECTION ( 'NONE',  ( 0.000000000000000000, -0.7071067811866525998, -0.7071067811864425456 ) ) ;
#4875 = VERTEX_POINT ( 'NONE', #2726 ) ;
#4876 = DIRECTION ( 'NONE',  ( 1.000000000000000000, 0.000000000000000000, 0.000000000000000000 ) ) ;
#4877 = DIRECTION ( 'NONE',  ( -1.000000000000000000, 0.000000000000000000, 0.000000000000000000 ) ) ;
#4878 = CARTESIAN_POINT ( 'NONE',  ( -4.000000000000000000, 24.80000000000000426, 2.309401076759000304 ) ) ;
#4879 = ORIENTED_EDGE ( 'NONE', *, *, #13460, .T. ) ;
#4880 = CARTESIAN_POINT ( 'NONE',  ( -18.81836685165999867, -9.538331588883998791, -0.2187837708677999871 ) ) ;
#4881 = CARTESIAN_POINT ( 'NONE',  ( -8.099999999999999645, -10.59999999999999964, 0.000000000000000000 ) ) ;
#4882 = CARTESIAN_POINT ( 'NONE',  ( 14.93427632872033151, 10.32886035222818144, 0.5993738056831997563 ) ) ;
#4883 = CARTESIAN_POINT ( 'NONE',  ( 24.39431354042982747, 9.829649394705615606, 2.587219325858395311E-05 ) ) ;
#4884 = AXIS2_PLACEMENT_3D ( 'NONE', #1117, #23642, #15992 ) ;
#4885 = CARTESIAN_POINT ( 'NONE',  ( 2.000000000000000000, 24.50000000000000000, 3.464101615137999968 ) ) ;
#4886 = CARTESIAN_POINT ( 'NONE',  ( 13.54033214797704510, 5.602808354962728110, -7.083871603166172370 ) ) ;
#4887 = CARTESIAN_POINT ( 'NONE',  ( -3.534157655880000082, 12.11469834677999735, -3.146902133593000528 ) ) ;
#4888 = EDGE_LOOP ( 'NONE', ( #4355, #18232, #17096 ) ) ;
#4889 = CIRCLE ( 'NONE', #19972, 13.77250448649000525 ) ;
#4890 = CARTESIAN_POINT ( 'NONE',  ( -13.03643231875999930, 10.05168146521000061, -2.584826834016999531 ) ) ;
#4891 = CARTESIAN_POINT ( 'NONE',  ( -1.653388338670852109, 29.31485580340598318, -1.389752403157769045 ) ) ;
#4892 = ORIENTED_EDGE ( 'NONE', *, *, #12504, .T. ) ;
#4893 = CARTESIAN_POINT ( 'NONE',  ( -5.833999999999999631, 1.296092693409999996E-14, 0.000000000000000000 ) ) ;
#4894 = CARTESIAN_POINT ( 'NONE',  ( -17.24117535985082839, -1.801531964190819846, -10.27922315481419879 ) ) ;
#4895 = EDGE_LOOP ( 'NONE', ( #20024, #22602, #8193, #8635, #18617, #17609 ) ) ;
#4896 = CARTESIAN_POINT ( 'NONE',  ( 5.087085786689997668, 13.95627596892002309, -4.275520105690998385 ) ) ;
#4897 = CARTESIAN_POINT ( 'NONE',  ( 1.709999999999999964, 9.000000000000000000, -0.3720215047547999476 ) ) ;
#4898 = CARTESIAN_POINT ( 'NONE',  ( 18.92995383753999761, -3.765411593996000228, 9.972057857162001326 ) ) ;
#4899 = EDGE_CURVE ( 'NONE', #17895, #744, #5045, .T. ) ;
#4900 = CARTESIAN_POINT ( 'NONE',  ( 16.81987658530999852, -0.9597138970337001362, 10.18860816546999892 ) ) ;
#4901 = ORIENTED_EDGE ( 'NONE', *, *, #18157, .F. ) ;
#4902 = AXIS2_PLACEMENT_3D ( 'NONE', #9585, #3663, #20498 ) ;
#4903 = B_SPLINE_CURVE_WITH_KNOTS ( 'NONE', 3,
 ( #16305, #5186, #7341, #18149, #12802, #1777, #22005, #23697, #18256, #14834 ),
 .UNSPECIFIED., .F., .F.,
 ( 4, 1, 1, 2, 2, 4 ),
 ( 0.000000000000000000, 0.2500000000000011102, 0.3750000000000014433, 0.4375000000000015543, 0.5000000000000016653, 1.000000000000000000 ),
 .UNSPECIFIED. ) ;
#4904 = CARTESIAN_POINT ( 'NONE',  ( -9.807316492921000162, 3.926761037699000312, 13.97645183750999998 ) ) ;
#4905 = AXIS2_PLACEMENT_3D ( 'NONE', #6681, #6929, #4761 ) ;
#4906 = CARTESIAN_POINT ( 'NONE',  ( 0.000000000000000000, 20.00000000000000000, 0.000000000000000000 ) ) ;
#4907 = ORIENTED_EDGE ( 'NONE', *, *, #10862, .F. ) ;
#4908 = DIRECTION ( 'NONE',  ( 0.000000000000000000, 1.000000000000000000, 0.000000000000000000 ) ) ;
#4909 = CARTESIAN_POINT ( 'NONE',  ( 24.50000000000000000, -8.246372141814999779, 6.625187740483999832 ) ) ;
#4910 = CARTESIAN_POINT ( 'NONE',  ( 16.37938660649435008, 3.607586543031612081, -9.735980039821285459 ) ) ;
#4911 = CARTESIAN_POINT ( 'NONE',  ( -5.212518166047371615, 14.09657958914241327, 5.244949423492627716 ) ) ;
#4912 = EDGE_CURVE ( 'NONE', #20571, #8904, #15923, .T. ) ;
#4913 = CARTESIAN_POINT ( 'NONE',  ( -14.49863740493600339, 11.08451042427808630, -5.800992024733025332 ) ) ;
#4914 = CONICAL_SURFACE ( 'NONE', #21915, 4.309401076758999416, 1.119376321708719590 ) ;
#4915 = CARTESIAN_POINT ( 'NONE',  ( -3.973605493815425049, 13.87927994308086177, -4.849889199551084218 ) ) ;
#4916 = DIRECTION ( 'NONE',  ( 1.000000000000000000, 0.000000000000000000, 0.000000000000000000 ) ) ;
#4917 = CARTESIAN_POINT ( 'NONE',  ( -2.015675766250876855, 30.15706052976086937, -0.7768981003585021528 ) ) ;
#4918 = ORIENTED_EDGE ( 'NONE', *, *, #16011, .T. ) ;
#4919 = CARTESIAN_POINT ( 'NONE',  ( -24.50000000000000000, 2.324045842668999493E-14, 12.50000000000000000 ) ) ;
#4920 = CARTESIAN_POINT ( 'NONE',  ( 20.85933913659999916, -10.86187836322000067, 0.5627353714132999896 ) ) ;
#4921 = CARTESIAN_POINT ( 'NONE',  ( 21.96499999999999986, -9.234946903777000671, 0.000000000000000000 ) ) ;
#4922 = AXIS2_PLACEMENT_3D ( 'NONE', #8284, #23040, #19429 ) ;
#4923 = CARTESIAN_POINT ( 'NONE',  ( -1.709420958921680223, 23.61501560995045779, -1.257455528530935229 ) ) ;
#4924 = ORIENTED_EDGE ( 'NONE', *, *, #19914, .T. ) ;
#4925 = CARTESIAN_POINT ( 'NONE',  ( -1.989999999999999991, 9.000000000000000000, 7.500000000000000000 ) ) ;
#4926 = CARTESIAN_POINT ( 'NONE',  ( 4.850875767706668285, 14.57047331221209241, 3.780275422591365508 ) ) ;
#4927 = CARTESIAN_POINT ( 'NONE',  ( 4.324670136826001432, 12.22299900889000313, -2.374696254288002795 ) ) ;
#4928 = EDGE_LOOP ( 'NONE', ( #20763, #18486, #18303, #13809 ) ) ;
#4929 = ADVANCED_FACE ( 'NONE', ( #22576 ), #11570, .T. ) ;
#4930 = CARTESIAN_POINT ( 'NONE',  ( -14.94905967094816290, 7.407576688393448627, -7.256950101879053427 ) ) ;
#4931 = CARTESIAN_POINT ( 'NONE',  ( 12.52688711657000020, -7.716878364870000340, -11.63397459621999985 ) ) ;
#4932 = EDGE_LOOP ( 'NONE', ( #16729, #5253, #1972, #10010 ) ) ;
#4933 = AXIS2_PLACEMENT_3D ( 'NONE', #2288, #574, #18757 ) ;
#4934 = CARTESIAN_POINT ( 'NONE',  ( 1.154873175401071261, 27.10110266264532797, 1.837081552305992016 ) ) ;
#4935 = DIRECTION ( 'NONE',  ( 0.000000000000000000, 0.000000000000000000, 1.000000000000000000 ) ) ;
#4936 = DIRECTION ( 'NONE',  ( 0.000000000000000000, 0.9998947838056817528, 0.01450590632083973396 ) ) ;
#4937 = EDGE_LOOP ( 'NONE', ( #23334, #671, #16910 ) ) ;
#4938 = CARTESIAN_POINT ( 'NONE',  ( 0.000000000000000000, 26.20000000000000284, -4.618802153517000519 ) ) ;
#4939 = VECTOR ( 'NONE', #10225, 1000.000000000000000 ) ;
#4940 = CARTESIAN_POINT ( 'NONE',  ( -3.644450799678000230, 14.33206891749000000, -4.922778709793999674 ) ) ;
#4941 = CARTESIAN_POINT ( 'NONE',  ( -19.40192413892000189, -10.54206147813000172, 0.0004700072724199000481 ) ) ;
#4942 = ADVANCED_FACE ( 'NONE', ( #19061 ), #4726, .T. ) ;
#4943 = CARTESIAN_POINT ( 'NONE',  ( -15.69524392073999941, 5.514258150326999619, -8.668746646227001307 ) ) ;
#4944 = CARTESIAN_POINT ( 'NONE',  ( -5.955309883888003419, 16.41439389789001524, 1.007156795900999935 ) ) ;
#4945 = B_SPLINE_CURVE_WITH_KNOTS ( 'NONE', 3,
 ( #769, #4664, #11927, #6592, #1012, #8414, #15899, #4410, #2590, #9979, #8169, #22924, #10104, #17491, #15653, #23044, #19558, #12049 ),
 .UNSPECIFIED., .F., .F.,
 ( 4, 2, 2, 2, 2, 2, 2, 2, 4 ),
 ( 0.000000000000000000, 0.1250000000000000555, 0.2500000000000001110, 0.3750000000000000555, 0.5000000000000000000, 0.6249999999999998890, 0.7499999999999998890, 0.8749999999999998890, 1.000000000000000000 ),
 .UNSPECIFIED. ) ;
#4946 = CARTESIAN_POINT ( 'NONE',  ( 15.59931994526000132, 7.986743723743999546, 6.465068481474999906 ) ) ;
#4947 = DIRECTION ( 'NONE',  ( 0.000000000000000000, -1.000000000000000000, 0.000000000000000000 ) ) ;
#4948 = CARTESIAN_POINT ( 'NONE',  ( -11.25088898725999975, -14.74911101273999847, 0.000000000000000000 ) ) ;
#4949 = CARTESIAN_POINT ( 'NONE',  ( 14.97354166666666231, -5.565137440292659221, -7.241319157828933761 ) ) ;
#4950 = EDGE_LOOP ( 'NONE', ( #3188, #298, #4521, #2106 ) ) ;
#4951 = CARTESIAN_POINT ( 'NONE',  ( -17.53780420454667777, 7.293940459210209504, 5.605577091469953643 ) ) ;
#4952 = LINE ( 'NONE', #17421, #21216 ) ;
#4953 = CARTESIAN_POINT ( 'NONE',  ( 1.812579491195999815, 27.54413313894999860, -1.675531247043999805 ) ) ;
#4954 = CIRCLE ( 'NONE', #18810, 1.399999999999999911 ) ;
#4955 = EDGE_CURVE ( 'NONE', #13125, #9013, #13607, .T. ) ;
#4956 = DIRECTION ( 'NONE',  ( -1.000000000000000000, 0.000000000000000000, 0.000000000000000000 ) ) ;
#4957 = CARTESIAN_POINT ( 'NONE',  ( -24.20553229332079326, 1.579827530622199605, -10.48222709070751080 ) ) ;
#4958 = CARTESIAN_POINT ( 'NONE',  ( -24.92272074369000023, -9.957998588256000261, -3.566033666137000235 ) ) ;
#4959 = CARTESIAN_POINT ( 'NONE',  ( -4.850000000102999920, 12.44999864901999942, -1.732907964652000048E-09 ) ) ;
#4960 = EDGE_LOOP ( 'NONE', ( #21615, #395, #5428 ) ) ;
#4961 = CARTESIAN_POINT ( 'NONE',  ( -3.644446339697000159, 14.33206891720999998, 4.922772686299000000 ) ) ;
#4962 = EDGE_CURVE ( 'NONE', #953, #18033, #19418, .T. ) ;
#4963 = CARTESIAN_POINT ( 'NONE',  ( 4.737384275571143277, 12.40724550023213979, -1.031760218791433648 ) ) ;
#4964 = CARTESIAN_POINT ( 'NONE',  ( -10.24501790109506771, 15.78861284533561360, 1.147143686903685289 ) ) ;
#4965 = CARTESIAN_POINT ( 'NONE',  ( 2.111585849641928192, 30.38130037447719900, 0.8546615592128204986 ) ) ;
#4966 = B_SPLINE_CURVE_WITH_KNOTS ( 'NONE', 3,
 ( #18681, #5949, #15840, #20616, #1073, #16853, #6642, #13783, #256, #11303, #7661, #21184, #4026, #4599, #19373, #10168, #11421, #18793 ),
 .UNSPECIFIED., .F., .F.,
 ( 4, 2, 2, 2, 2, 2, 2, 2, 4 ),
 ( 0.000000000000000000, 0.1250000000000000555, 0.2500000000000000555, 0.3750000000000000555, 0.5000000000000000000, 0.6249999999999998890, 0.7499999999999998890, 0.8749999999999998890, 1.000000000000000000 ),
 .UNSPECIFIED. ) ;
#4967 = CYLINDRICAL_SURFACE ( 'NONE', #4546, 3.000000000000000000 ) ;
#4968 = CARTESIAN_POINT ( 'NONE',  ( -16.48964823424000059, 10.66299948276999920, 3.938515806081000825 ) ) ;
#4969 = AXIS2_PLACEMENT_3D ( 'NONE', #21430, #15838, #4598 ) ;
#4970 = CARTESIAN_POINT ( 'NONE',  ( 14.05125142131000082, 6.790538403688000102, -6.859017754185999571 ) ) ;
#4971 = CARTESIAN_POINT ( 'NONE',  ( 18.97467215409325547, 0.8747362461518826127, 10.41931741152851565 ) ) ;
#4972 = ORIENTED_EDGE ( 'NONE', *, *, #20921, .T. ) ;
#4973 = EDGE_CURVE ( 'NONE', #11532, #15235, #8982, .T. ) ;
#4974 = CARTESIAN_POINT ( 'NONE',  ( -14.25243324638999809, 6.216878364870000340, 12.50000000000000000 ) ) ;
#4975 = CARTESIAN_POINT ( 'NONE',  ( 0.5408282081481999848, 29.08545613873999969, 2.669562448062999582 ) ) ;
#4976 = CARTESIAN_POINT ( 'NONE',  ( -14.70932910584000020, -9.048752088456000209, 0.000000000000000000 ) ) ;
#4977 = CARTESIAN_POINT ( 'NONE',  ( 3.665360768552284654, 14.33851491488757190, -4.911089631563983815 ) ) ;
#4978 = VERTEX_POINT ( 'NONE', #19316 ) ;
#4979 = DIRECTION ( 'NONE',  ( 1.000000000000000000, 0.000000000000000000, 0.000000000000000000 ) ) ;
#4980 = DIRECTION ( 'NONE',  ( 0.000000000000000000, -1.000000000000000000, 0.000000000000000000 ) ) ;
#4981 = CARTESIAN_POINT ( 'NONE',  ( 16.37183333333332058, -7.943906292456897944, 4.578726549357134523 ) ) ;
#4982 = CYLINDRICAL_SURFACE ( 'NONE', #17378, 2.500000000000000000 ) ;
#4983 = CARTESIAN_POINT ( 'NONE',  ( 16.06477897062039162, -0.5085830284804089274, -10.39831413926051340 ) ) ;
#4984 = CARTESIAN_POINT ( 'NONE',  ( -3.997397281504051492, 13.85564045854561144, 4.853569219738316676 ) ) ;
#4985 = CIRCLE ( 'NONE', #13863, 1.000000000000000000 ) ;
#4986 = CARTESIAN_POINT ( 'NONE',  ( 4.944937400867998711, 12.51442848420999177, -0.02374814528528999477 ) ) ;
#4987 = CARTESIAN_POINT ( 'NONE',  ( 20.43528936713000377, -9.195691514035999603, 0.000000000000000000 ) ) ;
#4988 = VERTEX_POINT ( 'NONE', #2475 ) ;
#4989 = DIRECTION ( 'NONE',  ( 0.000000000000000000, 0.000000000000000000, 1.000000000000000000 ) ) ;
#4990 = CARTESIAN_POINT ( 'NONE',  ( 1.712379611124581258, 12.94862384910287467, 1.057050596558879452 ) ) ;
#4991 = VECTOR ( 'NONE', #7255, 1000.000000000000000 ) ;
#4992 = EDGE_LOOP ( 'NONE', ( #18013, #7675, #19460, #14610 ) ) ;
#4993 = CARTESIAN_POINT ( 'NONE',  ( 2.665416330148000057, 24.43078970964999996, 0.6225038595752000470 ) ) ;
#4994 = EDGE_CURVE ( 'NONE', #7168, #15263, #15422, .T. ) ;
#4995 = CARTESIAN_POINT ( 'NONE',  ( 0.3272492347489618925, 28.45086340285666182, 2.499999999999996447 ) ) ;
#4996 = CARTESIAN_POINT ( 'NONE',  ( -12.06624327026013077, 1.367011989547999955E-14, 0.000000000000000000 ) ) ;
#4997 = EDGE_CURVE ( 'NONE', #15990, #3964, #5497, .T. ) ;
#4998 = B_SPLINE_CURVE_WITH_KNOTS ( 'NONE', 3,
 ( #2347, #12578, #9737, #22328, #17122, #7920, #19965, #10767, #22209, #14933, #18161, #1563, #8948, #5624, #21363, #10350, #4658, #19306 ),
 .UNSPECIFIED., .F., .F.,
 ( 4, 2, 2, 2, 2, 2, 2, 2, 4 ),
 ( 0.000000000000000000, 0.1250000000000000000, 0.2500000000000000000, 0.3750000000000000000, 0.4999999999999999445, 0.6250000000000000000, 0.7500000000000000000, 0.8750000000000000000, 1.000000000000000000 ),
 .UNSPECIFIED. ) ;
#4999 = CARTESIAN_POINT ( 'NONE',  ( 6.237174757059936070, 13.69932272150512986, -1.574127311046002564 ) ) ;
#5000 = LINE ( 'NONE', #12260, #10615 ) ;
#5001 = CARTESIAN_POINT ( 'NONE',  ( 5.699442596042000098, 1.405570106087591467E-14, 14.15464499511999996 ) ) ;
#5002 = ORIENTED_EDGE ( 'NONE', *, *, #10609, .F. ) ;
#5003 = AXIS2_PLACEMENT_3D ( 'NONE', #19478, #17659, #6870 ) ;
#5004 = CARTESIAN_POINT ( 'NONE',  ( -2.434931691670788378, 29.86753006952333678, 0.6543697108982053923 ) ) ;
#5005 = CARTESIAN_POINT ( 'NONE',  ( -1.212947244561992655, 26.21668223261122677, 1.752979114926064508 ) ) ;
#5006 = DIRECTION ( 'NONE',  ( 0.000000000000000000, -0.8660254037844288266, -0.5000000000000169864 ) ) ;
#5007 = ORIENTED_EDGE ( 'NONE', *, *, #9700, .T. ) ;
#5008 = EDGE_CURVE ( 'NONE', #7629, #16706, #7929, .T. ) ;
#5009 = CARTESIAN_POINT ( 'NONE',  ( -19.50383379408999929, 7.131897092901000157, 7.202928260512999614 ) ) ;
#5010 = DIRECTION ( 'NONE',  ( 0.7071067811823850136, -0.7071067811898851252, 1.080116765722976056E-06 ) ) ;
#5011 = CARTESIAN_POINT ( 'NONE',  ( 14.88774677762132548, 10.27520863958742225, -1.073445734337063362 ) ) ;
#5012 = AXIS2_PLACEMENT_3D ( 'NONE', #8164, #9294, #11108 ) ;
#5013 = DIRECTION ( 'NONE',  ( -1.000000000000000000, 0.000000000000000000, 0.000000000000000000 ) ) ;
#5014 = CARTESIAN_POINT ( 'NONE',  ( -0.8966937801068000091, 29.43620588595999976, 1.973860271291999702 ) ) ;
#5015 = CARTESIAN_POINT ( 'NONE',  ( -23.16929462096833703, 9.265295224643226746, 1.607743681355135241E-05 ) ) ;
#5016 = CARTESIAN_POINT ( 'NONE',  ( -2.674561911689002702, 11.95584864995998942, -3.929436066563998686 ) ) ;
#5017 = ORIENTED_EDGE ( 'NONE', *, *, #23568, .F. ) ;
#5018 = CARTESIAN_POINT ( 'NONE',  ( -1.074254588831038193, 26.46059486951026685, 2.123687106836487981 ) ) ;
#5019 = AXIS2_PLACEMENT_3D ( 'NONE', #12126, #19513, #10304 ) ;
#5020 = CARTESIAN_POINT ( 'NONE',  ( -1.503657042384516807, 29.30187328459274809, -1.552941005774420180 ) ) ;
#5021 = VERTEX_POINT ( 'NONE', #6470 ) ;
#5022 = CARTESIAN_POINT ( 'NONE',  ( 1.536366799937286087, 29.31666666666665932, -1.999167105995451665 ) ) ;
#5023 = CARTESIAN_POINT ( 'NONE',  ( -14.37619714886207589, -3.353739287365657074, 9.799118382956658380 ) ) ;
#5024 = AXIS2_PLACEMENT_3D ( 'NONE', #13684, #8497, #19264 ) ;
#5025 = EDGE_LOOP ( 'NONE', ( #14679, #19825 ) ) ;
#5026 = DIRECTION ( 'NONE',  ( 1.000000000000000000, 0.000000000000000000, 0.000000000000000000 ) ) ;
#5027 = CARTESIAN_POINT ( 'NONE',  ( 0.000000000000000000, 18.50000000000000000, 0.000000000000000000 ) ) ;
#5028 = CARTESIAN_POINT ( 'NONE',  ( 12.00000000000000000, -0.4784485517439919233, -8.984160855930003464 ) ) ;
#5029 = CARTESIAN_POINT ( 'NONE',  ( 17.03897356148999975, -6.252405066107000309, 9.153620030820999176 ) ) ;
#5030 = CARTESIAN_POINT ( 'NONE',  ( 12.98081408531000136, 6.028018288394999757, 8.144720004203000130 ) ) ;
#5031 = ORIENTED_EDGE ( 'NONE', *, *, #464, .T. ) ;
#5032 = CARTESIAN_POINT ( 'NONE',  ( -10.21460649291999978, 13.31930243424999993, -5.775538145385999300 ) ) ;
#5033 = DIRECTION ( 'NONE',  ( 0.000000000000000000, 0.000000000000000000, 1.000000000000000000 ) ) ;
#5034 = LINE ( 'NONE', #6704, #6431 ) ;
#5035 = CIRCLE ( 'NONE', #4235, 4.649999999999999467 ) ;
#5036 = EDGE_LOOP ( 'NONE', ( #10406, #21931, #8886, #14195, #20613 ) ) ;
#5037 = SURFACE_SIDE_STYLE ('',( #3337 ) ) ;
#5038 = PLANE ( 'NONE',  #10131 ) ;
#5039 = CARTESIAN_POINT ( 'NONE',  ( 23.14703506890763762, -6.420007756874271720, -8.432966434426246494 ) ) ;
#5040 = CARTESIAN_POINT ( 'NONE',  ( -5.771212219718563574, 15.14896488348015602, 2.962084404041542829 ) ) ;
#5042 = CARTESIAN_POINT ( 'NONE',  ( 16.27412392735353563, -0.09384471782549831664, -10.36545610267682349 ) ) ;
#5041 = CONICAL_SURFACE ( 'NONE', #10445, 2.249999993254999886, 0.7853981633972997312 ) ;
#5043 = CYLINDRICAL_SURFACE ( 'NONE', #6756, 11.50000000000000000 ) ;
#5044 = CARTESIAN_POINT ( 'NONE',  ( -2.036516393111000411, 31.06645568193000173, 0.5573742727589000578 ) ) ;
#5045 = B_SPLINE_CURVE_WITH_KNOTS ( 'NONE', 3,
 ( #4297, #9626, #4538, #5982, #13490, #2233, #20891, #23048, #13365, #891, #409, #13854, #9864, #17010, #21005, #17373, #21127, #11931 ),
 .UNSPECIFIED., .F., .F.,
 ( 4, 2, 2, 2, 2, 2, 2, 2, 4 ),
 ( 0.000000000000000000, 0.1250000000000000555, 0.2500000000000001110, 0.3750000000000001665, 0.5000000000000001110, 0.6250000000000001110, 0.7500000000000001110, 0.8750000000000000000, 1.000000000000000000 ),
 .UNSPECIFIED. ) ;
#5046 = LINE ( 'NONE', #3226, #4445 ) ;
#5047 = EDGE_CURVE ( 'NONE', #4023, #837, #13364, .T. ) ;
#5048 = CARTESIAN_POINT ( 'NONE',  ( -0.02483573736219273770, 30.00522634882376849, -2.170826557311644756 ) ) ;
#5049 = ORIENTED_EDGE ( 'NONE', *, *, #3881, .T. ) ;
#5050 = CARTESIAN_POINT ( 'NONE',  ( 18.78614059787999935, 2.403158705886000224, 10.26025450743999912 ) ) ;
#5051 = CARTESIAN_POINT ( 'NONE',  ( 23.27845441632221579, -8.182943452958516772, -6.730593103882281270 ) ) ;
#5052 = CARTESIAN_POINT ( 'NONE',  ( -1.445575777915792948, 23.61402273486993053, -1.544386912436334747 ) ) ;
#5053 = VERTEX_POINT ( 'NONE', #15902 ) ;
#5054 = CARTESIAN_POINT ( 'NONE',  ( -12.50000000000000000, 7.500000000000000000, 0.000000000000000000 ) ) ;
#5055 = CARTESIAN_POINT ( 'NONE',  ( 5.155702020191999857, 13.97328941143999970, -4.008166040501000893 ) ) ;
#5056 = CYLINDRICAL_SURFACE ( 'NONE', #10838, 13.93375672974000068 ) ;
#5057 = ORIENTED_EDGE ( 'NONE', *, *, #602, .T. ) ;
#5058 = CARTESIAN_POINT ( 'NONE',  ( 16.76700125730999957, -9.205641116351999997, -0.3944625347444000174 ) ) ;
#5059 = ORIENTED_EDGE ( 'NONE', *, *, #21937, .F. ) ;
#5060 = AXIS2_PLACEMENT_3D ( 'NONE', #20775, #9512, #15304 ) ;
#5061 = DIRECTION ( 'NONE',  ( -1.000000000000000000, 0.000000000000000000, 0.000000000000000000 ) ) ;
#5062 = DIRECTION ( 'NONE',  ( 1.000000000000000000, 0.000000000000000000, 0.000000000000000000 ) ) ;
#5063 = ORIENTED_EDGE ( 'NONE', *, *, #19030, .T. ) ;
#5064 = CARTESIAN_POINT ( 'NONE',  ( -10.04351714999000045, 16.35737901934999883, -1.000000000000000000 ) ) ;
#5065 = CARTESIAN_POINT ( 'NONE',  ( 12.12975174931000133, -10.21766741648000121, -2.893652579598999797 ) ) ;
#5066 = CARTESIAN_POINT ( 'NONE',  ( -19.72463381927000015, -10.05713679925000115, 1.864893016109999913 ) ) ;
#5067 = CARTESIAN_POINT ( 'NONE',  ( -17.72654740043000032, -1.911761373924000029, -10.15213107020000116 ) ) ;
#5068 = CARTESIAN_POINT ( 'NONE',  ( -1.670409819853669209, 24.49999999999984368, 3.654390594367815215 ) ) ;
#5069 = DIRECTION ( 'NONE',  ( 0.000000000000000000, 1.000000000000000000, 0.000000000000000000 ) ) ;
#5070 = CARTESIAN_POINT ( 'NONE',  ( -0.1402836262634008790, 27.99621943665322021, 2.168309435604789392 ) ) ;
#5071 = DIRECTION ( 'NONE',  ( -1.000000000000000000, 0.000000000000000000, 0.000000000000000000 ) ) ;
#5072 = ADVANCED_FACE ( 'NONE', ( #16019 ), #10229, .F. ) ;
#5073 = CARTESIAN_POINT ( 'NONE',  ( 15.57820833333332899, 9.071049241905111415, -1.187524516768772909 ) ) ;
#5074 = ORIENTED_EDGE ( 'NONE', *, *, #23157, .F. ) ;
#5075 = CARTESIAN_POINT ( 'NONE',  ( 23.61487358290123950, -0.1110235858477790771, 9.341576594489977126 ) ) ;
#5076 = PLANE ( 'NONE',  #23166 ) ;
#5077 = CARTESIAN_POINT ( 'NONE',  ( 1.884954223019000175, 28.21869850838000104, -1.259486242684000112 ) ) ;
#5078 = DIRECTION ( 'NONE',  ( 0.000000000000000000, 1.000000000000000000, 0.000000000000000000 ) ) ;
#5079 = CARTESIAN_POINT ( 'NONE',  ( -0.3356153332444000159, 27.99687716036000396, 2.426425728984999974 ) ) ;
#5080 = CARTESIAN_POINT ( 'NONE',  ( -4.745427439048141238, 12.41027624259845474, 0.9937658293378628382 ) ) ;
#5081 = ORIENTED_EDGE ( 'NONE', *, *, #11891, .T. ) ;
#5082 = DIRECTION ( 'NONE',  ( 0.000000000000000000, -1.000000000000000000, 0.000000000000000000 ) ) ;
#5083 = CARTESIAN_POINT ( 'NONE',  ( 3.041824996438589057, 11.87257502931641184, -3.747603760614300672 ) ) ;
#5084 = ADVANCED_FACE ( 'NONE', ( #19805 ), #22491, .F. ) ;
#5085 = CARTESIAN_POINT ( 'NONE',  ( -10.32545159102639687, 15.68979046979564629, 1.216685051509786897 ) ) ;
#5086 = CARTESIAN_POINT ( 'NONE',  ( 1.472041947694723518, 6.935496243266504379, 0.9522668941083732852 ) ) ;
#5087 = VERTEX_POINT ( 'NONE', #12295 ) ;
#5088 = CARTESIAN_POINT ( 'NONE',  ( -2.184465970885610009, 24.06666666666666643, 1.259047450927307521 ) ) ;
#5089 = DIRECTION ( 'NONE',  ( -1.000000000000000000, 0.000000000000000000, 0.000000000000000000 ) ) ;
#5090 = CARTESIAN_POINT ( 'NONE',  ( 13.61250142131000196, -6.495520710102000272, -7.123429297049000297 ) ) ;
#5091 = CARTESIAN_POINT ( 'NONE',  ( 18.58801564342164880, 10.31582294119393062, 1.512955792960317458 ) ) ;
#5092 = ORIENTED_EDGE ( 'NONE', *, *, #20156, .F. ) ;
#5093 = CARTESIAN_POINT ( 'NONE',  ( 2.184465970885645092, 28.46666666666667922, -1.259047450927249123 ) ) ;
#5094 = CARTESIAN_POINT ( 'NONE',  ( -2.686623376377999861, 29.68107362301000052, 0.4487213728548000158 ) ) ;
#5095 = CARTESIAN_POINT ( 'NONE',  ( 0.9652172239566000345, 23.62045304942999735, 2.538761913251999847 ) ) ;
#5096 = CARTESIAN_POINT ( 'NONE',  ( -4.850000000102999920, 12.44999864901999942, -1.732907964652000048E-09 ) ) ;
#5097 = ORIENTED_EDGE ( 'NONE', *, *, #8627, .T. ) ;
#5098 = CYLINDRICAL_SURFACE ( 'NONE', #1749, 7.000000000000000000 ) ;
#5099 = CARTESIAN_POINT ( 'NONE',  ( -24.50000000000000000, 10.82531754731000007, -6.250000000000000000 ) ) ;
#5100 = ADVANCED_FACE ( 'NONE', ( #19683 ), #23667, .T. ) ;
#5101 = DIRECTION ( 'NONE',  ( 0.000000000000000000, -1.000000000000000000, 0.000000000000000000 ) ) ;
#5102 = CARTESIAN_POINT ( 'NONE',  ( -23.74802958432387001, -8.939121534312308270, 3.416678463770061125 ) ) ;
#5103 = CARTESIAN_POINT ( 'NONE',  ( 16.03690177271507977, -1.513574074359952393, -10.29584712833434956 ) ) ;
#5104 = CARTESIAN_POINT ( 'NONE',  ( -4.122522811283552358, 13.74083509578544593, 4.883161027967257262 ) ) ;
#5105 = CARTESIAN_POINT ( 'NONE',  ( -0.1177307150814000253, 11.52529143281000756, 4.975641586845003239 ) ) ;
#5106 = CARTESIAN_POINT ( 'NONE',  ( -10.35615758860000035, 0.000000000000000000, 0.000000000000000000 ) ) ;
#5107 = ORIENTED_EDGE ( 'NONE', *, *, #346, .T. ) ;
#5108 = CARTESIAN_POINT ( 'NONE',  ( -4.080056528100000079, 26.50000000000000000, 4.563746053395999702 ) ) ;
#5109 = CARTESIAN_POINT ( 'NONE',  ( -4.000000000000000000, 26.47444252552741872, 0.7494995952805646455 ) ) ;
#5110 = ORIENTED_EDGE ( 'NONE', *, *, #13519, .F. ) ;
#5111 = CARTESIAN_POINT ( 'NONE',  ( 1.651019514586000048, 24.46469563812999937, -1.937031240432999901 ) ) ;
#5112 = CARTESIAN_POINT ( 'NONE',  ( 6.081503308973005950, 14.07691240018000123, -0.05979963850814000448 ) ) ;
#5113 = ADVANCED_FACE ( 'NONE', ( #21620 ), #5038, .T. ) ;
#5114 = CARTESIAN_POINT ( 'NONE',  ( -19.35893705290999733, -9.828989445528000246, 3.502754984265999738 ) ) ;
#5115 = CARTESIAN_POINT ( 'NONE',  ( -10.35615758860000035, 0.000000000000000000, 0.000000000000000000 ) ) ;
#5116 = CARTESIAN_POINT ( 'NONE',  ( -5.339884851010002542, 16.17859235010000418, -3.014934905543001697 ) ) ;
#5117 = CARTESIAN_POINT ( 'NONE',  ( 8.196152422706999729, 26.90192378864669820, -6.000000000000000000 ) ) ;
#5118 = ORIENTED_EDGE ( 'NONE', *, *, #11029, .F. ) ;
#5119 = CARTESIAN_POINT ( 'NONE',  ( -7.625774495095999583, 27.25000000000000000, 1.000000000000000000 ) ) ;
#5120 = CARTESIAN_POINT ( 'NONE',  ( -1.740327722686464851, 26.21338436845917741, 1.205708594814126844 ) ) ;
#5121 = CARTESIAN_POINT ( 'NONE',  ( 1.699999999999999956, 9.000014419210808470, 0.2828404724695334771 ) ) ;
#5122 = ORIENTED_EDGE ( 'NONE', *, *, #1441, .F. ) ;
#5123 = CARTESIAN_POINT ( 'NONE',  ( -20.26182243010999784, 5.856841114788999825, -8.930757166044001494 ) ) ;
#5124 = CARTESIAN_POINT ( 'NONE',  ( 23.99062354302999722, 7.716878364870000340, -11.63397459621999985 ) ) ;
#5125 = CARTESIAN_POINT ( 'NONE',  ( 15.09446924968909265, 8.461638818015519092, 5.944720952507684508 ) ) ;
#5126 = DIRECTION ( 'NONE',  ( -0.5000000000000169864, 0.000000000000000000, 0.8660254037844288266 ) ) ;
#5127 = CARTESIAN_POINT ( 'NONE',  ( 24.12589274536999895, -0.1537909274696999951, 11.30391051099999977 ) ) ;
#5128 = EDGE_CURVE ( 'NONE', #20342, #14322, #3017, .T. ) ;
#5129 = CARTESIAN_POINT ( 'NONE',  ( -1.143608723645000103, 30.12066899698000100, 2.065030851670000001 ) ) ;
#5130 = CARTESIAN_POINT ( 'NONE',  ( 13.60025666663938182, 6.914934984708120957, -5.791751039375853338 ) ) ;
#5131 = EDGE_CURVE ( 'NONE', #12555, #13009, #6306, .T. ) ;
#5132 = CARTESIAN_POINT ( 'NONE',  ( -2.096968522445999739, 11.83164223350000022, -4.269451356421001265 ) ) ;
#5133 = ORIENTED_EDGE ( 'NONE', *, *, #18366, .F. ) ;
#5134 = LINE ( 'NONE', #16484, #14493 ) ;
#5135 = ORIENTED_EDGE ( 'NONE', *, *, #21380, .T. ) ;
#5136 = DIRECTION ( 'NONE',  ( 1.000000000000000000, 0.000000000000000000, 0.000000000000000000 ) ) ;
#5137 = AXIS2_PLACEMENT_3D ( 'NONE', #3094, #17865, #1264 ) ;
#5138 = CYLINDRICAL_SURFACE ( 'NONE', #18490, 3.000000000000000000 ) ;
#5139 = ORIENTED_EDGE ( 'NONE', *, *, #6801, .F. ) ;
#5140 = CARTESIAN_POINT ( 'NONE',  ( -2.596700060712746172, 30.41537005277800887, 0.3120530614487230237 ) ) ;
#5141 = CARTESIAN_POINT ( 'NONE',  ( 2.228577735068977717, 30.71132486706381926, -0.6003337536057592461 ) ) ;
#5142 = EDGE_CURVE ( 'NONE', #5053, #2374, #2786, .T. ) ;
#5143 = CARTESIAN_POINT ( 'NONE',  ( -11.00000000000000000, 1.359357947053999856E-14, 0.000000000000000000 ) ) ;
#5144 = EDGE_CURVE ( 'NONE', #21343, #1360, #13449, .T. ) ;
#5145 = CARTESIAN_POINT ( 'NONE',  ( 15.41491548087999774, -10.50213854228000088, 3.406209761678000270 ) ) ;
#5146 = ORIENTED_EDGE ( 'NONE', *, *, #3353, .F. ) ;
#5147 = CARTESIAN_POINT ( 'NONE',  ( -11.74194399291999957, 12.57219865750999865, -7.259580034594999454 ) ) ;
#5148 = CARTESIAN_POINT ( 'NONE',  ( 13.50000000000000000, 8.460810473535371301, 5.109280266387623115 ) ) ;
#5149 = CARTESIAN_POINT ( 'NONE',  ( -14.49999963946489423, -11.08494587600286607, -5.800314632280170635 ) ) ;
#5150 = ORIENTED_EDGE ( 'NONE', *, *, #18394, .T. ) ;
#5151 = CARTESIAN_POINT ( 'NONE',  ( 11.48478210365700214, 12.46109695280949481, 3.416571976947520017 ) ) ;
#5152 = CARTESIAN_POINT ( 'NONE',  ( 20.85269734244679540, -7.751883840963948558, 7.131172731233752948 ) ) ;
#5153 = VECTOR ( 'NONE', #23146, 1000.000000000000000 ) ;
#5154 = CARTESIAN_POINT ( 'NONE',  ( -14.00000000000000000, 6.194304242614928846, 6.983547833180894671 ) ) ;
#5155 = CARTESIAN_POINT ( 'NONE',  ( 17.63245649294800188, -10.44981949161595480, 0.1351922335406884057 ) ) ;
#5156 = CARTESIAN_POINT ( 'NONE',  ( -18.44683259648000018, 8.205914313535998872, -7.494097690689000224 ) ) ;
#5157 = CARTESIAN_POINT ( 'NONE',  ( -1.997236045835000251, 31.07209288612999742, 0.9729124824121000437 ) ) ;
#5158 = CARTESIAN_POINT ( 'NONE',  ( -17.17989538244000158, -1.375580078895000113, 9.682594755839000200 ) ) ;
#5159 = CARTESIAN_POINT ( 'NONE',  ( 1.479086741115911874, 29.90763722216965448, -1.574257872583303408 ) ) ;
#5160 = VERTEX_POINT ( 'NONE', #4262 ) ;
#5161 = CARTESIAN_POINT ( 'NONE',  ( -23.97728971654375840, -5.151501961001863528, 12.49974207333311682 ) ) ;
#5162 = CARTESIAN_POINT ( 'NONE',  ( 19.36589339856000080, -11.12755619508000038, -2.338388569975000220 ) ) ;
#5163 = CARTESIAN_POINT ( 'NONE',  ( 2.000000000000000000, 30.00000000000000000, -3.464101615137999968 ) ) ;
#5164 = DIRECTION ( 'NONE',  ( 1.000000000000000000, 0.000000000000000000, 0.000000000000000000 ) ) ;
#5165 = ORIENTED_EDGE ( 'NONE', *, *, #20801, .F. ) ;
#5166 = FACE_OUTER_BOUND ( 'NONE', #21138, .T. ) ;
#5167 = DIRECTION ( 'NONE',  ( 0.000000000000000000, 0.000000000000000000, -1.000000000000000000 ) ) ;
#5168 = AXIS2_PLACEMENT_3D ( 'NONE', #6619, #10510, #10382 ) ;
#5169 = CARTESIAN_POINT ( 'NONE',  ( -2.759390417760998471, 11.76777182245000297, -3.989101613333998930 ) ) ;
#5170 = ORIENTED_EDGE ( 'NONE', *, *, #2920, .T. ) ;
#5171 = DIRECTION ( 'NONE',  ( -1.000000000000000000, 0.000000000000000000, 0.000000000000000000 ) ) ;
#5172 = ORIENTED_EDGE ( 'NONE', *, *, #14008, .T. ) ;
#5173 = DIRECTION ( 'NONE',  ( 0.000000000000000000, 1.000000000000000000, 0.000000000000000000 ) ) ;
#5174 = ITEM_DEFINED_TRANSFORMATION ( 'NONE', 'NONE', #9030,  #4390 ) ;
#5175 = DIRECTION ( 'NONE',  ( -1.000000000000000000, 4.163336342344362068E-12, 0.000000000000000000 ) ) ;
#5176 = PRODUCT_RELATED_PRODUCT_CATEGORY ( 'part', '', ( #483 ) ) ;
#5177 = ORIENTED_EDGE ( 'NONE', *, *, #18729, .F. ) ;
#5178 = CARTESIAN_POINT ( 'NONE',  ( -15.00576253787999903, -9.056359154562001024, 0.000000000000000000 ) ) ;
#5179 = CARTESIAN_POINT ( 'NONE',  ( -4.826881622125675619, 15.75359399380821657, -3.770934508614922187 ) ) ;
#5180 = CARTESIAN_POINT ( 'NONE',  ( -20.47403834912999798, 9.927636560707998825, 3.742326232843000255 ) ) ;
#5181 = CARTESIAN_POINT ( 'NONE',  ( -16.98007644595000087, -1.848015147739999975, 9.597958940837999720 ) ) ;
#5182 = CARTESIAN_POINT ( 'NONE',  ( -5.909536333224996163, 14.79956399133001810, -4.310204494228000449 ) ) ;
#5183 = CARTESIAN_POINT ( 'NONE',  ( -23.31517972632249780, -7.442898316286663096, 7.519379713872949011 ) ) ;
#5184 = CARTESIAN_POINT ( 'NONE',  ( -1.090060885945051128, 26.86992048250327514, -1.916741099986829955 ) ) ;
#5185 = FACE_OUTER_BOUND ( 'NONE', #9004, .T. ) ;
#5186 = CARTESIAN_POINT ( 'NONE',  ( -0.1784790855350541217, 29.74995697614779644, 4.515757205439222766 ) ) ;
#5187 = ORIENTED_EDGE ( 'NONE', *, *, #1258, .F. ) ;
#5188 = CYLINDRICAL_SURFACE ( 'NONE', #11480, 1.000000000000000222 ) ;
#5189 = FACE_OUTER_BOUND ( 'NONE', #16421, .T. ) ;
#5190 = CARTESIAN_POINT ( 'NONE',  ( -2.193530619437999984, 28.51119850838000147, -0.5724186824819998964 ) ) ;
#5191 = CONICAL_SURFACE ( 'NONE', #18706, 2.249999941723000330, 0.7853981633972997312 ) ;
#5192 = CARTESIAN_POINT ( 'NONE',  ( -24.44651966850621250, -6.713893699755834277, -8.217035123213300096 ) ) ;
#5193 = CARTESIAN_POINT ( 'NONE',  ( 0.4710401059126000378, 28.61614211382000050, 2.093446882794999908 ) ) ;
#5194 = CARTESIAN_POINT ( 'NONE',  ( -3.108885457403288921, 11.88968526009767501, 3.692999778167153746 ) ) ;
#5195 = ORIENTED_EDGE ( 'NONE', *, *, #17181, .T. ) ;
#5196 = CARTESIAN_POINT ( 'NONE',  ( -23.99212502906157951, -5.142273543674428460, -12.50000000000263434 ) ) ;
#5197 = CARTESIAN_POINT ( 'NONE',  ( -10.43398789387893011, 15.58306147486352877, 1.312348021278911148 ) ) ;
#5198 = CARTESIAN_POINT ( 'NONE',  ( -1.733098085964022372, 30.74034480246814738, -1.478422619745301869 ) ) ;
#5199 = VECTOR ( 'NONE', #22427, 1000.000000000000000 ) ;
#5200 = ORIENTED_EDGE ( 'NONE', *, *, #11048, .F. ) ;
#5201 = EDGE_CURVE ( 'NONE', #4666, #15717, #9742, .T. ) ;
#5202 = CARTESIAN_POINT ( 'NONE',  ( -1.999167105995410365, 24.08333333333333570, 1.536366799937339156 ) ) ;
#5203 = DIRECTION ( 'NONE',  ( -1.000000000000000000, 0.000000000000000000, 0.000000000000000000 ) ) ;
#5204 = B_SPLINE_CURVE_WITH_KNOTS ( 'NONE', 3,
 ( #1122, #22907, #17600, #994 ),
 .UNSPECIFIED., .F., .F.,
 ( 4, 4 ),
 ( 0.000000000000000000, 1.000000000000000000 ),
 .UNSPECIFIED. ) ;
#5205 = CARTESIAN_POINT ( 'NONE',  ( 12.29625142131000004, 8.002767958507000401, -5.312704480003000995 ) ) ;
#5206 = CARTESIAN_POINT ( 'NONE',  ( 18.70341255878536657, 8.877609467350925598, 5.471030932658075052 ) ) ;
#5207 = ORIENTED_EDGE ( 'NONE', *, *, #23608, .T. ) ;
#5208 = CARTESIAN_POINT ( 'NONE',  ( -24.41904027020412471, 2.048447027921860730, 12.49998758062118043 ) ) ;
#5209 = CARTESIAN_POINT ( 'NONE',  ( 13.50000000000000000, -4.865356088987999428, 9.073685197596999430 ) ) ;
#5210 = AXIS2_PLACEMENT_3D ( 'NONE', #166, #12789, #21875 ) ;
#5211 = CARTESIAN_POINT ( 'NONE',  ( -12.48432065477999942, 7.040382122447000235, -5.593108346885999005 ) ) ;
#5212 = CARTESIAN_POINT ( 'NONE',  ( 13.50000000000000178, -7.950673624646070969, 6.148396972236939817 ) ) ;
#5213 = ORIENTED_EDGE ( 'NONE', *, *, #7355, .T. ) ;
#5214 = CARTESIAN_POINT ( 'NONE',  ( -7.500000000000000000, 19.50000000000000000, -1.000000000000000000 ) ) ;
#5215 = DIRECTION ( 'NONE',  ( -1.000000000000000000, 0.000000000000000000, 0.000000000000000000 ) ) ;
#5216 = EDGE_CURVE ( 'NONE', #8248, #7244, #14001, .T. ) ;
#5217 = FACE_OUTER_BOUND ( 'NONE', #14177, .T. ) ;
#5218 = DIRECTION ( 'NONE',  ( -1.000000000000000000, 0.000000000000000000, 0.000000000000000000 ) ) ;
#5219 = CARTESIAN_POINT ( 'NONE',  ( -3.316314694148182696, 24.62756664670257933, 2.704122461039521141 ) ) ;
#5220 = CARTESIAN_POINT ( 'NONE',  ( 0.000000000000000000, 24.29999999999999716, 0.000000000000000000 ) ) ;
#5221 = CARTESIAN_POINT ( 'NONE',  ( -21.80950322054000168, 10.92268532154000127, 1.975424663057999908 ) ) ;
#5222 = VERTEX_POINT ( 'NONE', #22770 ) ;
#5223 = CARTESIAN_POINT ( 'NONE',  ( -2.500000000000000000, 18.50000000000000000, 0.000000000000000000 ) ) ;
#5224 = CARTESIAN_POINT ( 'NONE',  ( 1.670409819843222898, 24.49999999999985079, -3.654390594373847723 ) ) ;
#5225 = ORIENTED_EDGE ( 'NONE', *, *, #8833, .F. ) ;
#5226 = CARTESIAN_POINT ( 'NONE',  ( 1.286819792229999981, 25.02205787433999973, 2.195916730907999881 ) ) ;
#5227 = CARTESIAN_POINT ( 'NONE',  ( 2.504532394112000003E-14, 28.43419673618999965, 2.500000000000000000 ) ) ;
#5228 = CARTESIAN_POINT ( 'NONE',  ( 4.423870970800860114, 13.45434385453613935, 5.228893201776090294 ) ) ;
#5229 = CARTESIAN_POINT ( 'NONE',  ( 6.211427289479426683, 13.82660551420464401, -1.072280536642061799 ) ) ;
#5230 = CARTESIAN_POINT ( 'NONE',  ( -1.259047450927251566, 27.86666666666666714, -2.184465970885643316 ) ) ;
#5231 = EDGE_CURVE ( 'NONE', #367, #5021, #17730, .T. ) ;
#5232 = EDGE_LOOP ( 'NONE', ( #15308, #1682, #11181 ) ) ;
#5233 = DIRECTION ( 'NONE',  ( 0.000000000000000000, 0.000000000000000000, -1.000000000000000000 ) ) ;
#5234 = AXIS2_PLACEMENT_3D ( 'NONE', #23834, #5554, #5444 ) ;
#5235 = CARTESIAN_POINT ( 'NONE',  ( -1.972625189811084478, 26.24262259178813395, 0.8364124223001996317 ) ) ;
#5236 = DIRECTION ( 'NONE',  ( 1.000000000000000000, 0.000000000000000000, 0.000000000000000000 ) ) ;
#5237 = EDGE_LOOP ( 'NONE', ( #20410, #13794, #1778 ) ) ;
#5238 = CARTESIAN_POINT ( 'NONE',  ( -20.87476767895000052, -6.966064718177999993, 7.414690272311999841 ) ) ;
#5239 = CARTESIAN_POINT ( 'NONE',  ( 0.7782965750743000566, 25.53778480117000171, 1.998394996811000190 ) ) ;
#5240 = CARTESIAN_POINT ( 'NONE',  ( 14.45765107457843790, -0.1846454227282073313, -10.32464630637213610 ) ) ;
#5241 = CARTESIAN_POINT ( 'NONE',  ( 0.000000000000000000, 30.00000000000000000, 4.000000000000621725 ) ) ;
#5242 = CARTESIAN_POINT ( 'NONE',  ( 22.06995078665000065, 10.92978255278999811, 2.657704805107000023 ) ) ;
#5243 = CARTESIAN_POINT ( 'NONE',  ( -0.6418273050434999405, 30.72876582673999835, -2.070799230921999801 ) ) ;
#5244 = EDGE_CURVE ( 'NONE', #5087, #11168, #11673, .T. ) ;
#5245 = CARTESIAN_POINT ( 'NONE',  ( -22.67826950129917307, -1.210252803577252623, 9.252159271244858374 ) ) ;
#5246 = CARTESIAN_POINT ( 'NONE',  ( -6.528459799380125439, 15.44739108384869652, -1.496013491918405824 ) ) ;
#5247 = CARTESIAN_POINT ( 'NONE',  ( -1.704938782513197637, 26.34374313124272504, 1.466284411147575462 ) ) ;
#5248 = ORIENTED_EDGE ( 'NONE', *, *, #7422, .F. ) ;
#5249 = CARTESIAN_POINT ( 'NONE',  ( 0.6634078306992999829, 24.00000000000000000, -2.410371351092000403 ) ) ;
#5250 = CIRCLE ( 'NONE', #9113, 7.000000000000000000 ) ;
#5251 = FACE_OUTER_BOUND ( 'NONE', #19995, .T. ) ;
#5252 = ADVANCED_FACE ( 'NONE', ( #12494 ), #12382, .T. ) ;
#5253 = ORIENTED_EDGE ( 'NONE', *, *, #22531, .T. ) ;
#5254 = CARTESIAN_POINT ( 'NONE',  ( 16.93870833333332016, -1.192094632364749440, -9.105962353309886126 ) ) ;
#5255 = DIRECTION ( 'NONE',  ( -1.000000000000000000, 0.000000000000000000, 0.000000000000000000 ) ) ;
#5256 = CARTESIAN_POINT ( 'NONE',  ( 18.08784964760000236, 6.116917080091000436, -9.279135471629999188 ) ) ;
#5257 = EDGE_CURVE ( 'NONE', #10530, #11734, #10916, .T. ) ;
#5258 = ADVANCED_FACE ( 'NONE', ( #10559 ), #3055, .T. ) ;
#5259 = VERTEX_POINT ( 'NONE', #4869 ) ;
#5260 = CARTESIAN_POINT ( 'NONE',  ( -11.93084113877000085, 14.40041274848999997, 4.922277236253999710 ) ) ;
#5261 = DIRECTION ( 'NONE',  ( 1.000000000000000000, 0.000000000000000000, 0.000000000000000000 ) ) ;
#5262 = AXIS2_PLACEMENT_3D ( 'NONE', #12055, #2850, #15424 ) ;
#5263 = VERTEX_POINT ( 'NONE', #1226 ) ;
#5264 = CARTESIAN_POINT ( 'NONE',  ( 23.50001010374794319, 5.742227407948574225, -8.919603998024165037 ) ) ;
#5265 = CARTESIAN_POINT ( 'NONE',  ( -14.00000000000000355, 7.385559139612836610, 5.491114351475929745 ) ) ;
#5266 = CARTESIAN_POINT ( 'NONE',  ( 16.18747732770967929, -3.153525216371673157, -9.872168078842983974 ) ) ;
#5267 = CARTESIAN_POINT ( 'NONE',  ( -16.45953613113000102, 10.95060232793000132, -1.541397029415000119 ) ) ;
#5268 = CARTESIAN_POINT ( 'NONE',  ( 0.5475340434131998890, 30.78434480342999890, -2.278098825807999717 ) ) ;
#5269 = ADVANCED_FACE ( 'NONE', ( #21454 ), #23373, .T. ) ;
#5270 = CARTESIAN_POINT ( 'NONE',  ( -18.03317485555000133, 9.527592921995999831, -4.015252424095000272 ) ) ;
#5271 = CARTESIAN_POINT ( 'NONE',  ( 1.905473965356794031, 29.86637024958199760, -1.018015044609141162 ) ) ;
#5272 = ORIENTED_EDGE ( 'NONE', *, *, #1441, .T. ) ;
#5273 = CARTESIAN_POINT ( 'NONE',  ( 23.77835672501372599, -9.281039036324623126, -1.918975276430111748E-05 ) ) ;
#5274 = CARTESIAN_POINT ( 'NONE',  ( 19.36292747085767374, -10.00180209951941990, 3.178979607523860995 ) ) ;
#5275 = DIRECTION ( 'NONE',  ( -1.000000000000000000, 0.000000000000000000, 0.000000000000000000 ) ) ;
#5276 = ORIENTED_EDGE ( 'NONE', *, *, #17809, .T. ) ;
#5277 = CARTESIAN_POINT ( 'NONE',  ( 24.36414987671882315, -9.252522660948818256, -8.974160653052738468 ) ) ;
#5278 = CYLINDRICAL_SURFACE ( 'NONE', #13885, 2.000000000000000000 ) ;
#5279 = AXIS2_PLACEMENT_3D ( 'NONE', #3234, #10617, #9028 ) ;
#5280 = CARTESIAN_POINT ( 'NONE',  ( 3.165694020515001039, 11.93377496087999035, -3.621555223535997126 ) ) ;
#5281 = VERTEX_POINT ( 'NONE', #3295 ) ;
#5282 = EDGE_CURVE ( 'NONE', #19347, #10715, #6210, .T. ) ;
#5283 = CARTESIAN_POINT ( 'NONE',  ( 15.77981375731000036, 8.935760978467000015, -2.138706884349000248 ) ) ;
#5284 = ORIENTED_EDGE ( 'NONE', *, *, #14256, .T. ) ;
#5285 = CARTESIAN_POINT ( 'NONE',  ( 4.625000000000000000, 13.00000000000000000, 0.000000000000000000 ) ) ;
#5286 = CARTESIAN_POINT ( 'NONE',  ( -1.259047450927242462, 29.73333333333333783, 2.184465970885648201 ) ) ;
#5287 = ORIENTED_EDGE ( 'NONE', *, *, #7317, .T. ) ;
#5288 = CARTESIAN_POINT ( 'NONE',  ( -15.27030420454666881, -5.569817527973411231, 7.247409029951263015 ) ) ;
#5289 = CARTESIAN_POINT ( 'NONE',  ( -21.38556587436000100, -2.927468598044000281, -9.682091324420001754 ) ) ;
#5290 = CARTESIAN_POINT ( 'NONE',  ( -14.74564261827999978, -9.684186272450000743, -0.7343631782695000387 ) ) ;
#5292 = EDGE_CURVE ( 'NONE', #2748, #8374, #2753, .T. ) ;
#5291 = FACE_OUTER_BOUND ( 'NONE', #21435, .T. ) ;
#5293 = ADVANCED_FACE ( 'NONE', ( #1594 ), #4694, .F. ) ;
#5294 = CARTESIAN_POINT ( 'NONE',  ( -23.75267686402872513, 7.098219836623489876, 7.857347574748650310 ) ) ;
#5295 = CARTESIAN_POINT ( 'NONE',  ( -0.6568252240428453792, 26.36639859639442562, 2.105786140651809468 ) ) ;
#5296 = AXIS2_PLACEMENT_3D ( 'NONE', #21670, #4838, #23224 ) ;
#5297 = CARTESIAN_POINT ( 'NONE',  ( 0.000000000000000000, 22.19999999999999574, 0.000000000000000000 ) ) ;
#5298 = CARTESIAN_POINT ( 'NONE',  ( 14.70899999999999963, -9.048743642952000954, 0.000000000000000000 ) ) ;
#5299 = VERTEX_POINT ( 'NONE', #17705 ) ;
#5300 = CARTESIAN_POINT ( 'NONE',  ( 23.82624429608483752, -6.322309633054134181, 6.887171283258536114 ) ) ;
#5301 = PLANE ( 'NONE',  #12715 ) ;
#5302 = CARTESIAN_POINT ( 'NONE',  ( 13.90456468140257762, 7.335179754185822354, -5.351963236174892558 ) ) ;
#5303 = CARTESIAN_POINT ( 'NONE',  ( 6.124991240379277890, 14.37502773510814258, -0.3470611857344685913 ) ) ;
#5304 = CARTESIAN_POINT ( 'NONE',  ( -0.5776703561810999643, 26.06521896306000130, -2.213655236985999863 ) ) ;
#5305 = AXIS2_PLACEMENT_3D ( 'NONE', #15801, #12071, #12434 ) ;
#5306 = CARTESIAN_POINT ( 'NONE',  ( 61.60588651278290939, 37.01856778792605240, 6.000000000000000000 ) ) ;
#5307 = ORIENTED_EDGE ( 'NONE', *, *, #4070, .F. ) ;
#5308 = AXIS2_PLACEMENT_3D ( 'NONE', #3879, #2290, #11272 ) ;
#5309 = CARTESIAN_POINT ( 'NONE',  ( -0.5142367539521975894, 11.49354789453873771, -4.785507151825866501 ) ) ;
#5310 = CARTESIAN_POINT ( 'NONE',  ( -10.08844022186643308, 16.08101672535666538, 1.020213274384780711 ) ) ;
#5311 = VECTOR ( 'NONE', #9857, 1000.000000000000000 ) ;
#5312 = CARTESIAN_POINT ( 'NONE',  ( -20.93905420454666810, 1.205278475426004414, 9.208619112632755233 ) ) ;
#5313 = ORIENTED_EDGE ( 'NONE', *, *, #8949, .T. ) ;
#5314 = CARTESIAN_POINT ( 'NONE',  ( 0.000000000000000000, -1.550000000000000044, 0.000000000000000000 ) ) ;
#5315 = CARTESIAN_POINT ( 'NONE',  ( -15.91276253787999728, 9.079634562165001199, 0.000000000000000000 ) ) ;
#5316 = CARTESIAN_POINT ( 'NONE',  ( 18.43875142131000189, -2.600393254974000090, 9.414598814742999977 ) ) ;
#5317 = CARTESIAN_POINT ( 'NONE',  ( 18.45153449517520272, 9.899776480682962898, -3.255785108000626593 ) ) ;
#5318 = UNCERTAINTY_MEASURE_WITH_UNIT (LENGTH_MEASURE( 1.000000000000000082E-05 ), #6293, 'distance_accuracy_value', 'NONE');
#5319 = FACE_OUTER_BOUND ( 'NONE', #9179, .T. ) ;
#5320 = CARTESIAN_POINT ( 'NONE',  ( 0.8151085262080000060, 29.89420749509000075, -1.990313132251999795 ) ) ;
#5321 = DIRECTION ( 'NONE',  ( 0.000000000000000000, -1.000000000000000000, -1.361873576874000145E-14 ) ) ;
#5322 = CARTESIAN_POINT ( 'NONE',  ( 13.50000000000000355, -9.639306618178025587, 1.525625742284485220 ) ) ;
#5323 = AXIS2_PLACEMENT_3D ( 'NONE', #6555, #23374, #6669 ) ;
#5324 = ORIENTED_EDGE ( 'NONE', *, *, #13348, .T. ) ;
#5325 = PLANE ( 'NONE',  #5234 ) ;
#5326 = CARTESIAN_POINT ( 'NONE',  ( 21.71804314170000083, 2.151407657623999992, -11.09278661996000004 ) ) ;
#5327 = B_SPLINE_CURVE_WITH_KNOTS ( 'NONE', 3,
 ( #11513, #15237, #21064, #11747, #10056, #16951, #17439, #20707, #834, #7753 ),
 .UNSPECIFIED., .F., .F.,
 ( 4, 1, 1, 2, 2, 4 ),
 ( 0.000000000000000000, 0.2500000000000013323, 0.3750000000000016098, 0.4375000000000018874, 0.5000000000000021094, 1.000000000000000000 ),
 .UNSPECIFIED. ) ;
#5328 = CARTESIAN_POINT ( 'NONE',  ( 2.000000000000000000, 23.50000000000000000, 0.000000000000000000 ) ) ;
#5329 = AXIS2_PLACEMENT_3D ( 'NONE', #15452, #17648, #13635 ) ;
#5330 = FACE_OUTER_BOUND ( 'NONE', #11801, .T. ) ;
#5331 = CARTESIAN_POINT ( 'NONE',  ( -3.844548120735902685, 14.02704052081174169, 4.849063890147514044 ) ) ;
#5332 = CARTESIAN_POINT ( 'NONE',  ( 4.345815406654997659, 12.29811303589001170, 2.369899738314000359 ) ) ;
#5333 = ADVANCED_FACE ( 'NONE', ( #23255 ), #12641, .F. ) ;
#5334 = DIRECTION ( 'NONE',  ( 0.7071067811823850136, -0.7071067811898851252, 1.080116765722976056E-06 ) ) ;
#5335 = EDGE_LOOP ( 'NONE', ( #14982, #22305, #23844, #22797 ) ) ;
#5336 = DIRECTION ( 'NONE',  ( 0.000000000000000000, -1.000000000000000000, 0.000000000000000000 ) ) ;
#5337 = ORIENTED_EDGE ( 'NONE', *, *, #2920, .F. ) ;
#5338 = CARTESIAN_POINT ( 'NONE',  ( 2.104624887614000350, 24.11448581793999679, 0.4915318859118999462 ) ) ;
#5339 = CARTESIAN_POINT ( 'NONE',  ( 6.042541019908000521, 14.08632821477999642, 0.7169115693609001694 ) ) ;
#5340 = CARTESIAN_POINT ( 'NONE',  ( 11.48478210364558372, -3.271710350470782735, -12.49991250862539438 ) ) ;
#5341 = AXIS2_PLACEMENT_3D ( 'NONE', #22473, #4432, #22591 ) ;
#5342 = DIRECTION ( 'NONE',  ( 1.000000000000000000, 0.000000000000000000, 0.000000000000000000 ) ) ;
#5343 = ORIENTED_EDGE ( 'NONE', *, *, #20761, .F. ) ;
#5344 = CARTESIAN_POINT ( 'NONE',  ( -17.58615607838000372, 9.339993809354998788, 2.937842867551999859 ) ) ;
#5345 = B_SPLINE_CURVE_WITH_KNOTS ( 'NONE', 3,
 ( #791, #17764, #4559, #13996, #19580, #2746, #16040, #1167, #23064, #23196 ),
 .UNSPECIFIED., .F., .F.,
 ( 4, 2, 2, 2, 4 ),
 ( 0.000000000000000000, 0.1250000000000000000, 0.2500000000000000000, 0.5000000000000000000, 1.000000000000000000 ),
 .UNSPECIFIED. ) ;
#5346 = CARTESIAN_POINT ( 'NONE',  ( -1.922299668730066635, 26.22581021936841594, 0.9082030837895462838 ) ) ;
#5347 = PLANE ( 'NONE',  #1332 ) ;
#5348 = VERTEX_POINT ( 'NONE', #12839 ) ;
#5349 = CARTESIAN_POINT ( 'NONE',  ( -22.21937821538000080, 9.009440378489999901, -6.747651641374000420 ) ) ;
#5350 = CARTESIAN_POINT ( 'NONE',  ( 1.791338785401000111, 25.49639128499999785, 1.497938606261000061 ) ) ;
#5351 = CARTESIAN_POINT ( 'NONE',  ( 14.77023523311244801, 9.038162366719310725, -4.996207612869733694 ) ) ;
#5352 = CARTESIAN_POINT ( 'NONE',  ( -10.04281598263999875, 21.50000000000000000, -1.000000000000000000 ) ) ;
#5353 = CARTESIAN_POINT ( 'NONE',  ( 22.76721327243999937, -6.127619913867999202, 9.455514623800999274 ) ) ;
#5354 = FACE_OUTER_BOUND ( 'NONE', #4274, .T. ) ;
#5355 = CARTESIAN_POINT ( 'NONE',  ( 13.67356850472780749, 8.184989867075946890, -3.810691912912268275 ) ) ;
#5356 = CARTESIAN_POINT ( 'NONE',  ( -3.905562087987998421, 12.31943552251999208, -2.827962661607000605 ) ) ;
#5357 = AXIS2_PLACEMENT_3D ( 'NONE', #20341, #3749, #18523 ) ;
#5358 = CARTESIAN_POINT ( 'NONE',  ( -6.249999999202001000, 16.31160201366999729, 0.9999995866763998764 ) ) ;
#5359 = ADVANCED_FACE ( 'NONE', ( #13068 ), #1601, .T. ) ;
#5360 = VERTEX_POINT ( 'NONE', #3875 ) ;
#5361 = B_SPLINE_CURVE_WITH_KNOTS ( 'NONE', 3,
 ( #11826, #22595, #20550, #6002, #7714, #13627, #17400, #13386 ),
 .UNSPECIFIED., .F., .F.,
 ( 4, 2, 2, 4 ),
 ( 0.000000000000000000, 0.2500000000000000000, 0.5000000000000000000, 1.000000000000000000 ),
 .UNSPECIFIED. ) ;
#5362 = CARTESIAN_POINT ( 'NONE',  ( -14.98299556802001042, -9.055909390997985753, -0.7059549453755520343 ) ) ;
#5363 = CARTESIAN_POINT ( 'NONE',  ( 24.50000000000000711, -10.20789478510817183, 0.08277775137279635986 ) ) ;
#5364 = VERTEX_POINT ( 'NONE', #9558 ) ;
#5365 = AXIS2_PLACEMENT_3D ( 'NONE', #16481, #12856, #18211 ) ;
#5366 = CARTESIAN_POINT ( 'NONE',  ( -15.88087077250664336, 5.579446455848312780, -7.259938483122335029 ) ) ;
#5367 = CARTESIAN_POINT ( 'NONE',  ( 2.309807618587000011, 30.69019238141000017, -7.292675330123999428E-08 ) ) ;
#5368 = CARTESIAN_POINT ( 'NONE',  ( 0.000000000000000000, 2.449293598294999890E-14, 0.000000000000000000 ) ) ;
#5369 = VECTOR ( 'NONE', #22617, 1000.000000000000000 ) ;
#5370 = CONICAL_SURFACE ( 'NONE', #13083, 2.154903751016000069, 0.7853981633972997312 ) ;
#5371 = CARTESIAN_POINT ( 'NONE',  ( 15.59536637872000142, -10.51441018936999861, -3.384303748290000247 ) ) ;
#5372 = CARTESIAN_POINT ( 'NONE',  ( -15.56310688998895309, -10.21939891028472225, -2.520456394419640311 ) ) ;
#5373 = EDGE_CURVE ( 'NONE', #13184, #13716, #20890, .T. ) ;
#5374 = EDGE_LOOP ( 'NONE', ( #1008, #10067, #4041, #13334, #22335, #15780 ) ) ;
#5375 = CARTESIAN_POINT ( 'NONE',  ( -10.70897113876999995, 10.20678111663000109, -11.28814482413000064 ) ) ;
#5376 = AXIS2_PLACEMENT_3D ( 'NONE', #2648, #2772, #9172 ) ;
#5377 = CARTESIAN_POINT ( 'NONE',  ( 13.49999999999999645, 8.617162124728089623, -3.694302656813622576 ) ) ;
#5378 = CARTESIAN_POINT ( 'NONE',  ( -14.44633158889241287, -12.24656508597831994, -3.788310138431896235 ) ) ;
#5379 = ORIENTED_EDGE ( 'NONE', *, *, #17073, .F. ) ;
#5380 = CARTESIAN_POINT ( 'NONE',  ( 22.08810996438781871, 9.926075803855315627, 4.086635304993818885 ) ) ;
#5381 = CARTESIAN_POINT ( 'NONE',  ( 0.000000000000000000, -1.100000000000000089, 0.000000000000000000 ) ) ;
#5382 = CARTESIAN_POINT ( 'NONE',  ( 16.19333199072176299, -2.944109594543157460, -9.936999019503081954 ) ) ;
#5383 = EDGE_CURVE ( 'NONE', #6063, #4443, #7978, .T. ) ;
#5384 = DIRECTION ( 'NONE',  ( -6.465317295295811501E-08, 0.9999999999999703570, -2.351119575178930673E-07 ) ) ;
#5385 = VECTOR ( 'NONE', #10293, 1000.000000000000000 ) ;
#5386 = CARTESIAN_POINT ( 'NONE',  ( 2.192736427680999967, 30.56853374141000046, 0.8254858857236999636 ) ) ;
#5387 = CONICAL_SURFACE ( 'NONE', #2666, 2.249999993279999888, 0.7853981633972997312 ) ;
#5388 = CARTESIAN_POINT ( 'NONE',  ( -14.33607051085999906, 5.206569482801000071, -8.184903637703000001 ) ) ;
#5389 = EDGE_CURVE ( 'NONE', #13003, #9532, #15477, .T. ) ;
#5390 = CARTESIAN_POINT ( 'NONE',  ( 1.543414968236286988, 29.90237403121793491, -1.511123829192336343 ) ) ;
#5391 = VERTEX_POINT ( 'NONE', #20820 ) ;
#5392 = CARTESIAN_POINT ( 'NONE',  ( 0.9136931036111000104, 25.17769377914000017, -1.980922918787000109 ) ) ;
#5393 = CARTESIAN_POINT ( 'NONE',  ( 20.04388867876481939, 4.856218826689362444, -9.325685060479351307 ) ) ;
#5394 = CARTESIAN_POINT ( 'NONE',  ( -1.959792349063410599, 26.25942009138634603, 0.9068320924654740267 ) ) ;
#5395 = AXIS2_PLACEMENT_3D ( 'NONE', #18640, #16577, #1931 ) ;
#5396 = ORIENTED_EDGE ( 'NONE', *, *, #208, .T. ) ;
#5397 = DIRECTION ( 'NONE',  ( 0.000000000000000000, -0.7071067811866525998, -0.7071067811864425456 ) ) ;
#5398 = CARTESIAN_POINT ( 'NONE',  ( -6.180868275463003769, 14.99143150885001674, 3.733093067224003025 ) ) ;
#5399 = CARTESIAN_POINT ( 'NONE',  ( -4.762191296987998257, 12.38133858908998342, -1.240028857443999710 ) ) ;
#5400 = ORIENTED_EDGE ( 'NONE', *, *, #20478, .F. ) ;
#5401 = AXIS2_PLACEMENT_3D ( 'NONE', #7461, #3500, #10879 ) ;
#5402 = EDGE_CURVE ( 'NONE', #21964, #3898, #4415, .T. ) ;
#5403 = DIRECTION ( 'NONE',  ( 0.000000000000000000, 0.7071230553199298052, -0.7070905066786058457 ) ) ;
#5404 = ORIENTED_EDGE ( 'NONE', *, *, #13392, .T. ) ;
#5405 = VECTOR ( 'NONE', #18721, 1000.000000000000114 ) ;
#5406 = CARTESIAN_POINT ( 'NONE',  ( -4.183874459663874390, 15.15165427196963321, 4.473433887328480907 ) ) ;
#5407 = AXIS2_PLACEMENT_3D ( 'NONE', #1805, #209, #7132 ) ;
#5408 = CARTESIAN_POINT ( 'NONE',  ( -14.46758738532133748, -2.198682497502864042, -12.49996900093299779 ) ) ;
#5409 = VERTEX_POINT ( 'NONE', #17547 ) ;
#5410 = CARTESIAN_POINT ( 'NONE',  ( 23.08070603379666252, 9.022423395855687644, -2.424839258728616276 ) ) ;
#5411 = CARTESIAN_POINT ( 'NONE',  ( -20.26145907959000070, -4.462377008713000137, 9.043718231252999118 ) ) ;
#5412 = DIRECTION ( 'NONE',  ( 1.000000000000000000, 0.000000000000000000, 0.000000000000000000 ) ) ;
#5413 = CARTESIAN_POINT ( 'NONE',  ( -4.977206276429998688, 14.08710956103999123, -4.416616116876000753 ) ) ;
#5414 = CARTESIAN_POINT ( 'NONE',  ( -22.54312595389323093, 3.311030361751837070, -10.15954820832290828 ) ) ;
#5415 = CARTESIAN_POINT ( 'NONE',  ( 0.5334682286136585017, 28.03597116440634807, 2.139201694519461849 ) ) ;
#5416 = LINE ( 'NONE', #11101, #1537 ) ;
#5417 = EDGE_CURVE ( 'NONE', #7680, #1412, #16548, .T. ) ;
#5418 = CARTESIAN_POINT ( 'NONE',  ( 0.6642235200064005030, 30.76429554769410402, -2.063723317057710727 ) ) ;
#5419 = ORIENTED_EDGE ( 'NONE', *, *, #19027, .F. ) ;
#5420 = ADVANCED_FACE ( 'NONE', ( #11736, #17429 ), #18992, .T. ) ;
#5421 = CARTESIAN_POINT ( 'NONE',  ( -17.31105420454667154, 1.193091500503425273, 9.115517482220022671 ) ) ;
#5422 = CARTESIAN_POINT ( 'NONE',  ( 3.938926221699930785, 14.43711117119245912, 4.690475690813843634 ) ) ;
#5423 = CARTESIAN_POINT ( 'NONE',  ( 14.55789964817296678, -0.5615422284792254137, 9.079793271584962966 ) ) ;
#5424 = CARTESIAN_POINT ( 'NONE',  ( -14.25243324638999809, 13.93375672974000068, -0.8660254037843999608 ) ) ;
#5425 = CARTESIAN_POINT ( 'NONE',  ( 1.344743706340999934, 28.11271896306000073, 1.850881008969999852 ) ) ;
#5426 = CIRCLE ( 'NONE', #2712, 4.000000000000000000 ) ;
#5427 = CARTESIAN_POINT ( 'NONE',  ( 3.109386963286208783, 11.88982568152370511, 3.692506106354862538 ) ) ;
#5428 = ORIENTED_EDGE ( 'NONE', *, *, #16011, .F. ) ;
#5429 = CARTESIAN_POINT ( 'NONE',  ( -4.216012483316842641, 12.22071140417023827, -2.378417243159645533 ) ) ;
#5430 = EDGE_CURVE ( 'NONE', #17203, #5222, #18580, .T. ) ;
#5431 = DIRECTION ( 'NONE',  ( 0.000000000000000000, 1.000000000000000000, 0.000000000000000000 ) ) ;
#5432 = EDGE_CURVE ( 'NONE', #13113, #12315, #12427, .T. ) ;
#5433 = CARTESIAN_POINT ( 'NONE',  ( -4.000000000000000000, 28.30000000000000071, 2.309401076759000304 ) ) ;
#5434 = ORIENTED_EDGE ( 'NONE', *, *, #10594, .F. ) ;
#5435 = CARTESIAN_POINT ( 'NONE',  ( 0.1526552725783049125, 24.50000000000000000, 2.395140156181688074 ) ) ;
#5436 = CARTESIAN_POINT ( 'NONE',  ( -16.74417920454665420, -8.864047873708042147, -2.382277019715667521 ) ) ;
#5437 = CARTESIAN_POINT ( 'NONE',  ( 17.91675158530999923, 7.007286630565999985, -7.497846106583000214 ) ) ;
#5438 = CARTESIAN_POINT ( 'NONE',  ( 18.74522683489179897, 8.029184222409153193, 6.664625274391158705 ) ) ;
#5439 = CARTESIAN_POINT ( 'NONE',  ( 0.000000000000000000, 24.39999999221199900, -2.849999992212000066 ) ) ;
#5440 = CARTESIAN_POINT ( 'NONE',  ( 2.177130415331999913, 29.80110296423999827, 0.8625838095880999923 ) ) ;
#5441 = FACE_OUTER_BOUND ( 'NONE', #11137, .T. ) ;
#5442 = CARTESIAN_POINT ( 'NONE',  ( 13.50000000000000533, -9.258200915230130335, -2.291781170659658251 ) ) ;
#5443 = ORIENTED_EDGE ( 'NONE', *, *, #3558, .T. ) ;
#5444 = DIRECTION ( 'NONE',  ( 0.000000000000000000, -1.000000000000000000, 0.000000000000000000 ) ) ;
#5445 = CARTESIAN_POINT ( 'NONE',  ( 22.42623955032000183, 5.397027846906000015, 9.949281446147001162 ) ) ;
#5446 = CARTESIAN_POINT ( 'NONE',  ( -24.22578504060297533, 9.828293348740496427, 2.165122153287891926 ) ) ;
#5447 = CARTESIAN_POINT ( 'NONE',  ( 14.00186632564677858, -8.256169930635699927, -6.399381488568168130 ) ) ;
#5448 = DIRECTION ( 'NONE',  ( 0.000000000000000000, 0.000000000000000000, -1.000000000000000000 ) ) ;
#5449 = DIRECTION ( 'NONE',  ( -1.000000000000000000, 0.000000000000000000, 0.000000000000000000 ) ) ;
#5450 = CARTESIAN_POINT ( 'NONE',  ( -0.7774759188957669487, 29.25062229162126570, -2.015113548211680872 ) ) ;
#5451 = CARTESIAN_POINT ( 'NONE',  ( -22.47784140366999850, -5.954807860543000153, -9.388852349241998851 ) ) ;
#5452 = ORIENTED_EDGE ( 'NONE', *, *, #2886, .T. ) ;
#5453 = CARTESIAN_POINT ( 'NONE',  ( 2.385098070162194883, 23.88509807016325226, 0.2903665702034990415 ) ) ;
#5454 = ORIENTED_EDGE ( 'NONE', *, *, #8769, .F. ) ;
#5455 = CARTESIAN_POINT ( 'NONE',  ( -1.312395939795999888, 23.62679386126000125, -1.717109324558000027 ) ) ;
#5456 = CARTESIAN_POINT ( 'NONE',  ( 5.925473642861002865, 13.78915593935999517, 2.071179814652999163 ) ) ;
#5457 = CARTESIAN_POINT ( 'NONE',  ( 11.70388046502803192, 4.051054454412691186, -12.49994163047266760 ) ) ;
#5458 = FACE_OUTER_BOUND ( 'NONE', #17558, .T. ) ;
#5459 = CARTESIAN_POINT ( 'NONE',  ( 6.141065375610000210, 14.19649368052000149, -1.893142280157000292E-06 ) ) ;
#5460 = CARTESIAN_POINT ( 'NONE',  ( 19.00350174931000069, -5.312632942934000013, 9.204603991398000673 ) ) ;
#5461 = SHAPE_REPRESENTATION_RELATIONSHIP ( 'NONE' , 'NONE' ,  #22521, #3328 ) ;
#5462 = ORIENTED_EDGE ( 'NONE', *, *, #7923, .F. ) ;
#5463 = CARTESIAN_POINT ( 'NONE',  ( -14.53920085882999835, -1.325901587985999885, -9.615240848067001522 ) ) ;
#5464 = CARTESIAN_POINT ( 'NONE',  ( -2.750000000000000000, 22.19999999999999574, 0.000000000000000000 ) ) ;
#5465 = DIRECTION ( 'NONE',  ( -1.000000000000000000, 0.000000000000000000, 0.000000000000000000 ) ) ;
#5466 = VERTEX_POINT ( 'NONE', #22861 ) ;
#5467 = CARTESIAN_POINT ( 'NONE',  ( -20.50571085929999882, 6.147220618581999751, -9.373623392419000666 ) ) ;
#5468 = CARTESIAN_POINT ( 'NONE',  ( -2.110827410376000302, 24.51312697075000102, 0.3791487629745999843 ) ) ;
#5469 = CARTESIAN_POINT ( 'NONE',  ( 14.64207395721290084, 6.016812397516473787, -8.392094434179488971 ) ) ;
#5470 = CARTESIAN_POINT ( 'NONE',  ( 2.500000000000000000, 27.59999999999999787, 0.000000000000000000 ) ) ;
#5471 = CARTESIAN_POINT ( 'NONE',  ( 22.95076023539999710, -10.54968755136000169, 3.971415078648000474 ) ) ;
#5472 = FACE_OUTER_BOUND ( 'NONE', #4055, .T. ) ;
#5473 = CARTESIAN_POINT ( 'NONE',  ( 14.10175746976851130, 4.515222539071673147, 7.822146031336756344 ) ) ;
#5474 = CARTESIAN_POINT ( 'NONE',  ( -4.816593466898998699, 12.64429630393999027, -0.01116993232460000360 ) ) ;
#5475 = CARTESIAN_POINT ( 'NONE',  ( 12.00000000000000000, 5.273090321616999532, -7.267806174758000282 ) ) ;
#5476 = EDGE_LOOP ( 'NONE', ( #9949, #18667, #21393 ) ) ;
#5477 = CARTESIAN_POINT ( 'NONE',  ( -14.56584880966472717, -0.3730513441123999296, -9.047783283317706093 ) ) ;
#5478 = CARTESIAN_POINT ( 'NONE',  ( -14.05786623653591505, -10.40599112028010964, 1.415392338571896280 ) ) ;
#5479 = ORIENTED_EDGE ( 'NONE', *, *, #499, .F. ) ;
#5480 = LINE ( 'NONE', #20376, #8391 ) ;
#5481 = CARTESIAN_POINT ( 'NONE',  ( 1.373052545766183741, 30.76415608119967615, -1.788908248115641531 ) ) ;
#5482 = CARTESIAN_POINT ( 'NONE',  ( 12.00000000000000711, 4.679724461038802907, -7.698317349844846724 ) ) ;
#5483 = EDGE_CURVE ( 'NONE', #9495, #21993, #15706, .T. ) ;
#5484 = CARTESIAN_POINT ( 'NONE',  ( 19.22319703131000068, -3.768127178825000367, 9.979248983095997616 ) ) ;
#5485 = CARTESIAN_POINT ( 'NONE',  ( -14.27918997744984608, 0.2643314657130956813, 10.34628390161341116 ) ) ;
#5486 = CARTESIAN_POINT ( 'NONE',  ( -1.500144717171000064, 28.04419433609999857, -2.447990496630999768 ) ) ;
#5487 = ORIENTED_EDGE ( 'NONE', *, *, #15103, .F. ) ;
#5488 = CARTESIAN_POINT ( 'NONE',  ( -9.690746138770000684, -14.59218309192000085, -4.320739656328999700 ) ) ;
#5489 = CARTESIAN_POINT ( 'NONE',  ( 13.50000000000000178, 7.080145657724991715, 7.062653394649239580 ) ) ;
#5490 = CARTESIAN_POINT ( 'NONE',  ( -14.25243324638999809, -7.716878364870000340, 11.63397459621999985 ) ) ;
#5491 = EDGE_CURVE ( 'NONE', #23570, #17036, #21318, .T. ) ;
#5492 = ORIENTED_EDGE ( 'NONE', *, *, #14088, .T. ) ;
#5493 = CARTESIAN_POINT ( 'NONE',  ( 23.58825386245753819, 8.156183226283769017, -6.776067362772733027 ) ) ;
#5494 = CARTESIAN_POINT ( 'NONE',  ( 0.000000000000000000, 22.19999999999999574, 0.000000000000000000 ) ) ;
#5495 = CARTESIAN_POINT ( 'NONE',  ( 16.00713081564376594, -8.311260887379887663, -6.185970973389042449 ) ) ;
#5496 = CARTESIAN_POINT ( 'NONE',  ( -15.37555624093999995, -9.817107509510000440, -5.025949249001999242 ) ) ;
#5497 = CIRCLE ( 'NONE', #2002, 2.899999999999999911 ) ;
#5498 = CARTESIAN_POINT ( 'NONE',  ( 1.651614159710000029, 28.91398226591000054, 1.661872489819000043 ) ) ;
#5499 = CARTESIAN_POINT ( 'NONE',  ( -17.62691415960999919, 5.507581498160999622, 8.736692431694999428 ) ) ;
#5500 = EDGE_CURVE ( 'NONE', #5602, #23303, #2776, .T. ) ;
#5501 = CARTESIAN_POINT ( 'NONE',  ( 2.155981317445319512, 29.81398103993711857, -0.1719232382127588998 ) ) ;
#5502 = VERTEX_POINT ( 'NONE', #13658 ) ;
#5503 = CARTESIAN_POINT ( 'NONE',  ( -2.310215611903000177, 23.83319443196000265, 0.3439361960344000102 ) ) ;
#5504 = CARTESIAN_POINT ( 'NONE',  ( 21.15045064161181898, -9.711026941284815805, 4.098456068966175536 ) ) ;
#5505 = DIRECTION ( 'NONE',  ( 0.000000000000000000, 0.000000000000000000, -1.000000000000000000 ) ) ;
#5506 = B_SPLINE_CURVE_WITH_KNOTS ( 'NONE', 3,
 ( #6006, #4566, #19210, #13881, #18853, #6369, #9886, #15203, #6248, #15682, #11477, #11597, #18969, #13631, #17275, #8082, #4083, #2259, #15449, #8198, #22600, #9652, #21027, #4440, #13393, #11830, #9767, #17153, #7954, #15324, #6127, #10016, #17405, #15566, #13752, #21152, #11957, #22716, #2752, #19344, #10133, #17522, #916, #8316, #15810, #12556, #1174, #3240, #23319, #23203, #18132, #14003, #10381, #6734, #17772, #4934, #8807, #16048, #2871, #16169, #15926, #4811, #8926, #1413, #6617, #8443, #3124, #8566, #23686, #23440, #7093, #23572, #21284, #12080, #19942, #3362, #14126, #10255, #21397, #12198, #10741, #14368, #16292, #8682, #19587 ),
 .UNSPECIFIED., .F., .F.,
 ( 4, 2, 2, 2, 2, 2, 2, 2, 2, 2, 2, 2, 2, 2, 2, 2, 2, 1, 2, 2, 2, 2, 2, 1, 2, 2, 2, 2, 2, 1, 2, 2, 2, 2, 2, 2, 2, 2, 2, 2, 2, 2, 2, 4 ),
 ( 0.000000000000000000, 0.01232754932072391285, 0.02465509864144782570, 0.04931019728289567222, 0.07396529592434351874, 0.09862039456579137220, 0.1109479438865152712, 0.1232754932072391979, 0.1479305918486870375, 0.1725856904901348909, 0.1972407891315827444, 0.2095683384523066572, 0.2218958877730305423, 0.2465509864144784513, 0.2712060850559263048, 0.2958611836973741305, 0.3081887330180980711, 0.3205162823388220117, 0.3328438316595459523, 0.3451713809802698374, 0.3698264796217177186, 0.3944815782631655443, 0.4068091275838894849, 0.4191366769046134255, 0.4314642262253373661, 0.4437917755460611957, 0.4684468741875091324, 0.4931019728289570692, 0.5054295221496809543, 0.5177570714704048394, 0.5300846207911287244, 0.5424121701118527206, 0.5670672687533004908, 0.5917223673947482609, 0.6163774660361961422, 0.6287050153569201383, 0.6410325646776440234, 0.6656876633190919046, 0.6903427619605397858, 0.7149978606019877780, 0.7273254099227116631, 0.7396529592434355482, 0.7643080578848834294, 0.7889631565263313107 ),
 .UNSPECIFIED. ) ;
#5507 = ORIENTED_EDGE ( 'NONE', *, *, #1371, .F. ) ;
#5508 = CARTESIAN_POINT ( 'NONE',  ( 0.000000000000000000, 20.00000000000000000, 0.000000000000000000 ) ) ;
#5509 = CARTESIAN_POINT ( 'NONE',  ( 0.000000000000000000, -1.550000000000000044, 0.000000000000000000 ) ) ;
#5510 = CARTESIAN_POINT ( 'NONE',  ( 4.726723308362996256, 12.38017690019999861, -1.078906772315999296 ) ) ;
#5511 = EDGE_LOOP ( 'NONE', ( #19915, #3439, #877, #4892 ) ) ;
#5512 = CARTESIAN_POINT ( 'NONE',  ( 13.14731375731000007, -9.095564035174998452, -0.6525005121013000009 ) ) ;
#5513 = ORIENTED_EDGE ( 'NONE', *, *, #23275, .F. ) ;
#5514 = DIRECTION ( 'NONE',  ( 1.000000000000000000, 0.000000000000000000, 0.000000000000000000 ) ) ;
#5515 = APPLICATION_PROTOCOL_DEFINITION ( 'draft international standard', 'automotive_design', 1998, #4320 ) ;
#5516 = CARTESIAN_POINT ( 'NONE',  ( 2.000000000000000000, 18.89999999999999858, 5.041407240605999832E-11 ) ) ;
#5517 = EDGE_CURVE ( 'NONE', #21669, #11307, #15488, .T. ) ;
#5518 = VERTEX_POINT ( 'NONE', #8224 ) ;
#5519 = CARTESIAN_POINT ( 'NONE',  ( -23.50032910583999879, -5.270462733209999584, -7.631233524726999562 ) ) ;
#5520 = CARTESIAN_POINT ( 'NONE',  ( 12.00000000000000000, -3.609001420916660319, -8.868091556110934803 ) ) ;
#5521 = CARTESIAN_POINT ( 'NONE',  ( 11.70388046502923096, -8.799739770593536292, -9.758286884884382673 ) ) ;
#5522 = CARTESIAN_POINT ( 'NONE',  ( 18.71491666666665310, -2.395514397407730200, -8.913304601090439760 ) ) ;
#5523 = CARTESIAN_POINT ( 'NONE',  ( -23.52106073230301320, -0.7157372019101019278, 10.55885782059828593 ) ) ;
#5524 = CARTESIAN_POINT ( 'NONE',  ( 0.6162257440955131171, 27.24093660882355650, 2.118443747156355084 ) ) ;
#5525 = DIRECTION ( 'NONE',  ( 0.000000000000000000, 0.000000000000000000, -1.000000000000000000 ) ) ;
#5526 = CARTESIAN_POINT ( 'NONE',  ( -5.934366589030004135, 15.81056974690001837, 1.225118323253999275 ) ) ;
#5527 = EDGE_CURVE ( 'NONE', #8899, #2037, #10878, .T. ) ;
#5528 = CARTESIAN_POINT ( 'NONE',  ( 2.137480853478654019, 30.62211454086312656, -0.3111734527053177657 ) ) ;
#5529 = ORIENTED_EDGE ( 'NONE', *, *, #3850, .T. ) ;
#5530 = DIRECTION ( 'NONE',  ( 0.000000000000000000, -1.000000000000000000, 0.000000000000000000 ) ) ;
#5531 = CARTESIAN_POINT ( 'NONE',  ( 13.50000000000000000, -4.002954420673999536, -8.080569262580000967 ) ) ;
#5532 = AXIS2_PLACEMENT_3D ( 'NONE', #1598, #17836, #23742 ) ;
#5533 = CARTESIAN_POINT ( 'NONE',  ( -20.99236729085494702, -10.09761506543422804, -2.944074382273693224 ) ) ;
#5534 = CARTESIAN_POINT ( 'NONE',  ( 2.236906829057999868, 25.78687716036000310, 0.5033195914047999819 ) ) ;
#5535 = CARTESIAN_POINT ( 'NONE',  ( -14.00000000000000000, 1.396097351027999937E-14, 0.000000000000000000 ) ) ;
#5536 = ORIENTED_EDGE ( 'NONE', *, *, #1771, .F. ) ;
#5537 = ADVANCED_FACE ( 'NONE', ( #2401 ), #9709, .T. ) ;
#5538 = CARTESIAN_POINT ( 'NONE',  ( -4.585468453814590006, 12.35085399519005911, -1.572948697367331006 ) ) ;
#5539 = CARTESIAN_POINT ( 'NONE',  ( -2.900806500513820829, 29.93562577624027909, 2.944020739578861789 ) ) ;
#5540 = CARTESIAN_POINT ( 'NONE',  ( -19.10482910584000038, 1.458613477275000161E-14, 0.000000000000000000 ) ) ;
#5541 = EDGE_LOOP ( 'NONE', ( #17408, #12788, #16808, #10611 ) ) ;
#5542 = EDGE_CURVE ( 'NONE', #12558, #22774, #74, .T. ) ;
#5543 = EDGE_CURVE ( 'NONE', #13895, #23303, #8161, .T. ) ;
#5544 = CARTESIAN_POINT ( 'NONE',  ( -23.75390978279000009, 13.93375672974000068, 0.5776826028407999747 ) ) ;
#5545 = CARTESIAN_POINT ( 'NONE',  ( -0.6543697108981931798, 28.16666666666667140, 2.434931691670791043 ) ) ;
#5546 = CARTESIAN_POINT ( 'NONE',  ( 16.16175158531000022, 8.345400111538999965, -5.893156809269999741 ) ) ;
#5547 = CARTESIAN_POINT ( 'NONE',  ( 18.05781943074418550, -1.146451644013575244, -10.34773016139448032 ) ) ;
#5548 = CARTESIAN_POINT ( 'NONE',  ( -24.17970357213072319, 4.108081272002125139, 12.49999456974980561 ) ) ;
#5549 = CARTESIAN_POINT ( 'NONE',  ( -1.502772323173000135, 29.33784492091999851, -1.796001945673999955 ) ) ;
#5550 = DIRECTION ( 'NONE',  ( 0.000000000000000000, -0.9761919106981273853, 0.2169086293524060682 ) ) ;
#5551 = CARTESIAN_POINT ( 'NONE',  ( 13.50000000000000000, -9.000981082165885994, 4.172073181103733930 ) ) ;
#5552 = ORIENTED_EDGE ( 'NONE', *, *, #2376, .F. ) ;
#5553 = AXIS2_PLACEMENT_3D ( 'NONE', #9012, #22193, #11186 ) ;
#5554 = DIRECTION ( 'NONE',  ( 0.000000000000000000, 0.000000000000000000, -1.000000000000000000 ) ) ;
#5555 = CARTESIAN_POINT ( 'NONE',  ( 19.41640481369000071, -11.20635663128000203, -0.8231659222257999842 ) ) ;
#5556 = EDGE_CURVE ( 'NONE', #18434, #629, #20091, .T. ) ;
#5557 = CARTESIAN_POINT ( 'NONE',  ( -9.000000000000000000, 19.50000000000000000, -6.000000000000000000 ) ) ;
#5558 = ORIENTED_EDGE ( 'NONE', *, *, #22567, .T. ) ;
#5559 = ADVANCED_FACE ( 'NONE', ( #18850 ), #16276, .T. ) ;
#5560 = CARTESIAN_POINT ( 'NONE',  ( 24.50000000000000355, -5.730830435609104434, 8.891180258077504561 ) ) ;
#5561 = CARTESIAN_POINT ( 'NONE',  ( 0.000000000000000000, 24.65000000674550051, 0.000000000000000000 ) ) ;
#5562 = CARTESIAN_POINT ( 'NONE',  ( -4.283717669607001177, 12.21694329250999367, 2.261528323867997958 ) ) ;
#5563 = CARTESIAN_POINT ( 'NONE',  ( -0.7577245197952828804, 29.24939092660360629, -2.022592451772749378 ) ) ;
#5564 = CARTESIAN_POINT ( 'NONE',  ( -20.13865776273999941, 10.50400506863999972, -3.445110567144999525 ) ) ;
#5565 = ORIENTED_EDGE ( 'NONE', *, *, #5244, .T. ) ;
#5566 = CARTESIAN_POINT ( 'NONE',  ( 0.000000000000000000, 18.10000000000000142, 0.000000000000000000 ) ) ;
#5567 = ORIENTED_EDGE ( 'NONE', *, *, #14863, .F. ) ;
#5568 = CIRCLE ( 'NONE', #8285, 12.44999999999999929 ) ;
#5569 = CARTESIAN_POINT ( 'NONE',  ( 2.113544220839000065, 25.71690224701999838, 0.4514181673775000125 ) ) ;
#5570 = CARTESIAN_POINT ( 'NONE',  ( 6.232327572681000127, 13.71183716028998845, 0.7484834382456998503 ) ) ;
#5571 = CARTESIAN_POINT ( 'NONE',  ( -19.55887123173999953, -9.833822427806001798, 3.504477313184999776 ) ) ;
#5572 = CARTESIAN_POINT ( 'NONE',  ( 0.000000000000000000, 20.00000000000000000, 0.000000000000000000 ) ) ;
#5573 = CARTESIAN_POINT ( 'NONE',  ( 23.99062354302999722, -13.93375672974000068, 0.8660254037843999608 ) ) ;
#5574 = CARTESIAN_POINT ( 'NONE',  ( 17.72381424930999927, -7.480404092888999656, -7.743571870822999692 ) ) ;
#5575 = CONICAL_SURFACE ( 'NONE', #12915, 3.049999825846000157, 0.7853981633972997312 ) ;
#5576 = ORIENTED_EDGE ( 'NONE', *, *, #6427, .F. ) ;
#5577 = CARTESIAN_POINT ( 'NONE',  ( -16.36737399056000086, -1.805578197078999914, -9.588658350757999216 ) ) ;
#5578 = DIRECTION ( 'NONE',  ( 0.000000000000000000, 1.000000000000000000, 0.000000000000000000 ) ) ;
#5579 = ORIENTED_EDGE ( 'NONE', *, *, #16595, .T. ) ;
#5580 = CARTESIAN_POINT ( 'NONE',  ( -10.29403125534151009, 15.72585302211925296, -1.189404080594516078 ) ) ;
#5581 = CARTESIAN_POINT ( 'NONE',  ( 2.063368671964000090, 25.70856110624000124, -0.2979541432074999663 ) ) ;
#5582 = CARTESIAN_POINT ( 'NONE',  ( 14.40569269110591577, -1.986665269285088797, -10.12885916003707898 ) ) ;
#5583 = CARTESIAN_POINT ( 'NONE',  ( 0.000000000000000000, 9.000000000000000000, 0.000000000000000000 ) ) ;
#5584 = CARTESIAN_POINT ( 'NONE',  ( 23.46447575822000076, -6.913963705398000315, -8.920945031365000943 ) ) ;
#5585 = CARTESIAN_POINT ( 'NONE',  ( 0.5079312758524999749, 28.61268239940000058, 2.305192271312999974 ) ) ;
#5586 = ADVANCED_FACE ( 'NONE', ( #5888 ), #13965, .T. ) ;
#5587 = CARTESIAN_POINT ( 'NONE',  ( 13.70021229750822123, 8.494204404046966417, -3.039004686995299132 ) ) ;
#5588 = DIRECTION ( 'NONE',  ( -1.000000000000000000, 0.000000000000000000, 0.000000000000000000 ) ) ;
#5589 = CARTESIAN_POINT ( 'NONE',  ( -6.737757365823932254, 15.34323595062688206, 1.749766658884769344 ) ) ;
#5590 = CARTESIAN_POINT ( 'NONE',  ( 21.68490460127999953, 4.300247781276000048, -10.59540847689999943 ) ) ;
#5591 = ORIENTED_EDGE ( 'NONE', *, *, #4369, .F. ) ;
#5592 = CARTESIAN_POINT ( 'NONE',  ( -14.62564808937985994, -2.249539402723780945, -8.791895681600211176 ) ) ;
#5593 = CARTESIAN_POINT ( 'NONE',  ( 12.12543434882657323, -13.45291906885515409, 1.698934468806285514 ) ) ;
#5594 = ORIENTED_EDGE ( 'NONE', *, *, #23599, .T. ) ;
#5595 = CARTESIAN_POINT ( 'NONE',  ( -2.121106334292000017, 30.87889366360999688, 6.284935476095000148E-07 ) ) ;
#5596 = CARTESIAN_POINT ( 'NONE',  ( 23.99062354302999722, 7.716878364870000340, 11.63397459621999985 ) ) ;
#5597 = CARTESIAN_POINT ( 'NONE',  ( 21.41787270046332026, 8.980959603804187452, 2.413435494101626499 ) ) ;
#5598 = CIRCLE ( 'NONE', #14107, 10.30000000000000071 ) ;
#5599 = CARTESIAN_POINT ( 'NONE',  ( 18.92244553490999692, 7.034701712467999357, 8.633984044295999638 ) ) ;
#5600 = CARTESIAN_POINT ( 'NONE',  ( -6.225913922104028053, 15.76757470349466139, 1.159797651207155944 ) ) ;
#5601 = CARTESIAN_POINT ( 'NONE',  ( 1.099251314038999894, 28.53962896666999782, 2.157402177123000087 ) ) ;
#5602 = VERTEX_POINT ( 'NONE', #6004 ) ;
#5603 = AXIS2_PLACEMENT_3D ( 'NONE', #13440, #17199, #7998 ) ;
#5604 = CARTESIAN_POINT ( 'NONE',  ( -11.83639256584999977, 14.79789546886000018, -1.442137029629999789 ) ) ;
#5605 = LINE ( 'NONE', #20617, #14024 ) ;
#5606 = CARTESIAN_POINT ( 'NONE',  ( -14.49863740983932558, -10.56606202787202164, -6.698971014606366126 ) ) ;
#5607 = ORIENTED_EDGE ( 'NONE', *, *, #23001, .T. ) ;
#5608 = CARTESIAN_POINT ( 'NONE',  ( -24.36724102300186701, 9.545677019765191673, 8.466242377950417008 ) ) ;
#5609 = CARTESIAN_POINT ( 'NONE',  ( 18.91133465082729614, -3.947989545138891998, 9.718486893964049855 ) ) ;
#5610 = CARTESIAN_POINT ( 'NONE',  ( 23.99062354302999722, 13.93375672974000068, 0.8660254037843999608 ) ) ;
#5611 = CARTESIAN_POINT ( 'NONE',  ( 15.92946909780416220, -9.691739620817704903, -3.655258532792393211 ) ) ;
#5612 = CARTESIAN_POINT ( 'NONE',  ( -18.92073910527999914, 2.264199207268999814, -10.89315635654000047 ) ) ;
#5613 = CARTESIAN_POINT ( 'NONE',  ( -1.901161826014999834, 30.05505061217000318, 1.092502442907999916 ) ) ;
#5614 = AXIS2_PLACEMENT_3D ( 'NONE', #12120, #8486, #23488 ) ;
#5615 = CARTESIAN_POINT ( 'NONE',  ( -16.20500172382000059, 9.665285290698001575, -3.525418390172999850 ) ) ;
#5616 = CARTESIAN_POINT ( 'NONE',  ( 1.797367992752552990, 29.72859529399798006, 1.204889009139612055 ) ) ;
#5617 = EDGE_LOOP ( 'NONE', ( #8988, #22154, #1245, #14646, #3239, #12009, #16635, #21819 ) ) ;
#5618 = CARTESIAN_POINT ( 'NONE',  ( 2.133148737088000235, 25.80587366863000298, 0.4564637253469999711 ) ) ;
#5619 = CARTESIAN_POINT ( 'NONE',  ( 20.95183695597172147, -4.891656435019153371, 9.332274347635205913 ) ) ;
#5620 = LINE ( 'NONE', #21751, #6451 ) ;
#5621 = ORIENTED_EDGE ( 'NONE', *, *, #20208, .T. ) ;
#5622 = EDGE_CURVE ( 'NONE', #20307, #8984, #7633, .T. ) ;
#5623 = CARTESIAN_POINT ( 'NONE',  ( 2.500000000000000444, 30.25634700817417766, -0.4349195733711135325 ) ) ;
#5624 = CARTESIAN_POINT ( 'NONE',  ( 17.61895833333332462, 7.295785356393542642, 5.606677399942485707 ) ) ;
#5625 = CARTESIAN_POINT ( 'NONE',  ( 12.70856375730999943, -1.114725866925000197, 9.038927914362998806 ) ) ;
#5626 = ORIENTED_EDGE ( 'NONE', *, *, #10251, .F. ) ;
#5627 = AXIS2_PLACEMENT_3D ( 'NONE', #1685, #9073, #16446 ) ;
#5628 = CARTESIAN_POINT ( 'NONE',  ( -3.931174283351645204, 14.83584528699218552, 4.702583796344565137 ) ) ;
#5629 = CARTESIAN_POINT ( 'NONE',  ( -14.48875654244861089, 1.295999377426451771, -12.49999522859631185 ) ) ;
#5630 = VERTEX_POINT ( 'NONE', #14684 ) ;
#5631 = CARTESIAN_POINT ( 'NONE',  ( 22.28708103379667804, -9.243212137893149105, -1.209806691843604343 ) ) ;
#5632 = CARTESIAN_POINT ( 'NONE',  ( 2.259444391955999443, 11.86379749507999648, 4.184941550337999416 ) ) ;
#5633 = CARTESIAN_POINT ( 'NONE',  ( -22.13650671462999853, -8.888489588850999823, 3.669257322618999950 ) ) ;
#5634 = CARTESIAN_POINT ( 'NONE',  ( -13.73165055702999915, 8.564239710418998897, -4.480696141197999971 ) ) ;
#5635 = CARTESIAN_POINT ( 'NONE',  ( -21.38504529524956510, -9.746759242728279204, 3.986291022453713584 ) ) ;
#5636 = FACE_OUTER_BOUND ( 'NONE', #6420, .T. ) ;
#5637 = CARTESIAN_POINT ( 'NONE',  ( 16.25845833333332990, -5.585221661844576246, 7.267866498838181144 ) ) ;
#5638 = DIRECTION ( 'NONE',  ( 0.000000000000000000, 0.000000000000000000, -1.000000000000000000 ) ) ;
#5639 = CARTESIAN_POINT ( 'NONE',  ( 1.399078845269212223, 30.71403437281561111, -1.645507438231223363 ) ) ;
#5640 = ORIENTED_EDGE ( 'NONE', *, *, #20635, .F. ) ;
#5641 = CARTESIAN_POINT ( 'NONE',  ( -17.69487077250666829, 5.608054106645548487, -7.297163626529473035 ) ) ;
#5642 = CARTESIAN_POINT ( 'NONE',  ( 0.000000000000000000, 22.00000000000000000, 0.000000000000000000 ) ) ;
#5643 = LINE ( 'NONE', #22350, #5405 ) ;
#5644 = VECTOR ( 'NONE', #20196, 1000.000000000000000 ) ;
#5645 = EDGE_CURVE ( 'NONE', #12531, #7629, #17520, .T. ) ;
#5646 = CARTESIAN_POINT ( 'NONE',  ( -24.07165041821819784, 6.096641539000005494, -8.671681623059738442 ) ) ;
#5647 = CARTESIAN_POINT ( 'NONE',  ( -1.950678319476999878, 26.16271896306000144, -1.195388535980999922 ) ) ;
#5648 = DIRECTION ( 'NONE',  ( -0.4226182617407191477, 0.000000000000000000, 0.9063077870366409439 ) ) ;
#5649 = CARTESIAN_POINT ( 'NONE',  ( 3.083557478243028172, 11.88318476793270584, 3.713866788134294605 ) ) ;
#5650 = VERTEX_POINT ( 'NONE', #15807 ) ;
#5651 = CARTESIAN_POINT ( 'NONE',  ( 0.4544561634010835793, 11.49156783371328849, -4.790238354834232659 ) ) ;
#5652 = CARTESIAN_POINT ( 'NONE',  ( 24.00034722001000276, -6.716786535997999685, -12.21137788282999992 ) ) ;
#5653 = CARTESIAN_POINT ( 'NONE',  ( -1.844810972989856968, 29.95044706087815456, -1.336380754565594797 ) ) ;
#5654 = ORIENTED_EDGE ( 'NONE', *, *, #2299, .F. ) ;
#5655 = ADVANCED_FACE ( 'NONE', ( #14000 ), #14006, .F. ) ;
#5656 = CARTESIAN_POINT ( 'NONE',  ( 23.41677564524290744, 34.01856778792605240, -115.0195023120000002 ) ) ;
#5657 = CIRCLE ( 'NONE', #4511, 4.625000000000000000 ) ;
#5658 = VECTOR ( 'NONE', #20898, 1000.000000000000000 ) ;
#5659 = CARTESIAN_POINT ( 'NONE',  ( 14.29706408530999973, 7.153286345558000470, -7.225396115407999531 ) ) ;
#5660 = CARTESIAN_POINT ( 'NONE',  ( 18.33301707778365497, 7.724375581193626772, -6.994159490549959557 ) ) ;
#5661 = CARTESIAN_POINT ( 'NONE',  ( -4.000000000000000000, 28.30000000000000071, 2.309401076759000304 ) ) ;
#5662 = CARTESIAN_POINT ( 'NONE',  ( -1.725915770149999862, 30.22510609745999943, 1.283340576838000180 ) ) ;
#5663 = DIRECTION ( 'NONE',  ( 0.000000000000000000, 1.000000000000000000, 0.000000000000000000 ) ) ;
#5664 = CARTESIAN_POINT ( 'NONE',  ( 13.50000000000000178, -8.365255057625532231, -4.267281750524336559 ) ) ;
#5665 = ORIENTED_EDGE ( 'NONE', *, *, #5500, .T. ) ;
#5666 = EDGE_CURVE ( 'NONE', #21240, #14252, #22461, .T. ) ;
#5667 = CARTESIAN_POINT ( 'NONE',  ( -2.499999999999999556, 28.81666666666666643, 0.3272492347489436848 ) ) ;
#5668 = CARTESIAN_POINT ( 'NONE',  ( 21.45820040743999968, -10.73102562442999819, 0.8320772051962000981 ) ) ;
#5669 = DIRECTION ( 'NONE',  ( 0.1671082301074949539, 0.9859385576344705804, 0.000000000000000000 ) ) ;
#5670 = ORIENTED_EDGE ( 'NONE', *, *, #18187, .F. ) ;
#5671 = CARTESIAN_POINT ( 'NONE',  ( 24.50000000000000000, -5.821110578647480160, 8.832467286812930141 ) ) ;
#5672 = CARTESIAN_POINT ( 'NONE',  ( 2.000000000000000000, 28.00000000000000000, 3.464101615137999968 ) ) ;
#5673 = CARTESIAN_POINT ( 'NONE',  ( 1.648798782356001080, 11.55618995303000496, 4.569391161061998829 ) ) ;
#5674 = AXIS2_PLACEMENT_3D ( 'NONE', #22834, #20915, #675 ) ;
#5675 = CARTESIAN_POINT ( 'NONE',  ( -0.7657973753844729004, 29.24989338039968700, -2.019557259306400177 ) ) ;
#5676 = EDGE_CURVE ( 'NONE', #1912, #5222, #9307, .T. ) ;
#5677 = CARTESIAN_POINT ( 'NONE',  ( -12.24999999999999822, 10.00898580939830218, -10.96118423669926756 ) ) ;
#5678 = ORIENTED_EDGE ( 'NONE', *, *, #14230, .F. ) ;
#5679 = FACE_BOUND ( 'NONE', #20973, .T. ) ;
#5680 = EDGE_LOOP ( 'NONE', ( #23833, #1710, #1579, #18476, #13818, #22129 ) ) ;
#5681 = CARTESIAN_POINT ( 'NONE',  ( -0.5998269938833999948, 25.50789140844999991, 2.076358161442000139 ) ) ;
#5682 = CARTESIAN_POINT ( 'NONE',  ( 5.373436897387995792, 13.85347760506000192, 3.916935352515997781 ) ) ;
#5683 = DIRECTION ( 'NONE',  ( 0.000000000000000000, -1.000000000000000000, 0.000000000000000000 ) ) ;
#5684 = CARTESIAN_POINT ( 'NONE',  ( 15.97587270046332542, 8.844941937541273447, 2.376881761915226488 ) ) ;
#5685 = CARTESIAN_POINT ( 'NONE',  ( -7.500000000000000000, -9.000000000000000000, 0.000000000000000000 ) ) ;
#5686 = CARTESIAN_POINT ( 'NONE',  ( 24.00034722001000276, -13.93375672974000068, -0.2887811715185000239 ) ) ;
#5687 = DIRECTION ( 'NONE',  ( 0.000000000000000000, -1.000000000000000000, 0.000000000000000000 ) ) ;
#5688 =( LENGTH_UNIT ( ) NAMED_UNIT ( * ) SI_UNIT ( .MILLI., .METRE. ) );
#5689 = EDGE_CURVE ( 'NONE', #14083, #2875, #20325, .T. ) ;
#5690 = CARTESIAN_POINT ( 'NONE',  ( -18.39867747026000089, -7.918532069388001027, -5.797808426274999150 ) ) ;
#5691 = AXIS2_PLACEMENT_3D ( 'NONE', #10046, #10410, #17431 ) ;
#5692 = CARTESIAN_POINT ( 'NONE',  ( 4.000000000000000000, 29.87418302490049626, 1.506880184559475255 ) ) ;
#5693 = CARTESIAN_POINT ( 'NONE',  ( -14.29262089130507363, 5.684429818794539457, 12.49999999999983658 ) ) ;
#5694 = ORIENTED_EDGE ( 'NONE', *, *, #3460, .T. ) ;
#5695 = CARTESIAN_POINT ( 'NONE',  ( -23.07621189342000179, -10.06116254826999956, 5.098950990742999956 ) ) ;
#5696 = CARTESIAN_POINT ( 'NONE',  ( 0.6079502603517000781, 24.15152788257999816, -2.254560651513999758 ) ) ;
#5697 = CARTESIAN_POINT ( 'NONE',  ( 14.55979580643064963, 3.396064661906295523, -9.748015653831131999 ) ) ;
#5698 = CARTESIAN_POINT ( 'NONE',  ( -17.87792920454667467, 7.977774763500829813, -4.597956546261363187 ) ) ;
#5699 = CARTESIAN_POINT ( 'NONE',  ( 19.68384026807999732, -1.917285116153000013, -11.01718559352000071 ) ) ;
#5700 = CIRCLE ( 'NONE', #19238, 12.44999999999999929 ) ;
#5701 = CARTESIAN_POINT ( 'NONE',  ( -0.3657044282044999428, 28.56480980899999977, 2.248360111627000002 ) ) ;
#5702 = CARTESIAN_POINT ( 'NONE',  ( 13.69887155650829058, 8.480249914508103615, -3.077469453800580013 ) ) ;
#5703 = CARTESIAN_POINT ( 'NONE',  ( 2.352846606927001538, 11.89851893293999652, -4.242708344949997823 ) ) ;
#5704 = CARTESIAN_POINT ( 'NONE',  ( -6.216900810347000039, 16.31160418525000111, 0.9999988273041999776 ) ) ;
#5705 = ADVANCED_FACE ( 'NONE', ( #5441 ), #9187, .F. ) ;
#5706 = CARTESIAN_POINT ( 'NONE',  ( 11.32654380052400178, 9.540497826158469863, -8.475313523008512817 ) ) ;
#5707 = ORIENTED_EDGE ( 'NONE', *, *, #18366, .T. ) ;
#5708 = EDGE_CURVE ( 'NONE', #6198, #6330, #11258, .T. ) ;
#5709 = CARTESIAN_POINT ( 'NONE',  ( 2.403644530880252539, 23.90364453088029961, -0.2598880820672725966 ) ) ;
#5710 = CIRCLE ( 'NONE', #6493, 7.500000000000000000 ) ;
#5711 = MECHANICAL_DESIGN_GEOMETRIC_PRESENTATION_REPRESENTATION (  '', ( #16148 ), #16920 ) ;
#5712 = ORIENTED_EDGE ( 'NONE', *, *, #7026, .T. ) ;
#5713 = B_SPLINE_SURFACE_WITH_KNOTS ( 'NONE', 3, 3, ( 
 ( #20468, #7618, #11269, #6031, #22505, #2052, #22392, #14880, #5915, #6158, #17059, #16816, #3876, #13543, #14994, #15110, #11385, #22267, #13187, #7859, #5805, #13299, #3990, #9679, #18756, #2166, #9559, #18879, #13420, #341, #20698, #4231, #7743, #2287, #4106 ),
 ( #11505, #457, #22623, #11624, #18993, #2402, #9793, #18101, #20151, #3559, #23286, #14091, #14218, #1259, #8647, #3208, #10592, #17978, #1380, #8772, #14685, #9241, #14909, #14792, #5718, #1851, #18443, #18677, #5945, #20731, #22188, #16727, #1736, #20503, #9353 ),
 ( #5601, #1970, #11180, #4137, #7411, #20612, #137, #13332, #2083, #11535, #23887, #16618, #7776, #12982, #9123, #16496, #18566, #22428, #9473, #12866, #22078, #16976, #11057, #27, #2199, #3909, #20382, #15143, #3790, #22540, #7528, #22303, #13105, #11300, #16850 ),
 ( #253, #7293, #7658, #11417, #15030, #5486, #20266, #18789, #3669, #5835, #13219, #4021, #9591, #377, #21337, #17333, #10195, #13695, #979, #9711, #13454, #22895, #17462, #23135, #737, #10076, #609, #4753, #18914, #17094, #856, #6310, #4631, #20857, #17212 ) ),
 .UNSPECIFIED., .F., .F., .F.,
 ( 4, 4 ),
 ( 4, 1, 1, 1, 1, 1, 1, 1, 1, 1, 1, 1, 1, 1, 1, 1, 1, 1, 1, 1, 1, 1, 1, 1, 1, 1, 1, 1, 1, 1, 1, 1, 4 ),
 ( -0.3056682515952000023, 1.305668251594999996 ),
 ( -0.02000000000000000042, 0.01250000000000000069, 0.04499999999999999833, 0.07749999999999999944, 0.1100000000000000006, 0.1424999999999999878, 0.1749999999999999889, 0.2074999999999999900, 0.2399999999999999911, 0.2725000000000000200, 0.3049999999999999933, 0.3375000000000000222, 0.3699999999999999956, 0.4025000000000000244, 0.4349999999999999978, 0.4675000000000000266, 0.5000000000000000000, 0.5324999999999999734, 0.5649999999999999467, 0.5975000000000000311, 0.6300000000000000044, 0.6624999999999999778, 0.6949999999999999512, 0.7275000000000000355, 0.7600000000000000089, 0.7924999999999999822, 0.8249999999999999556, 0.8575000000000000400, 0.8900000000000000133, 0.9224999999999999867, 0.9549999999999999600, 0.9875000000000000444, 1.020000000000000018 ),
 .UNSPECIFIED. ) ;
#5714 = DIRECTION ( 'NONE',  ( 0.000000000000000000, -1.000000000000000000, 0.000000000000000000 ) ) ;
#5715 = CARTESIAN_POINT ( 'NONE',  ( -8.035714285714000482, 1.323055916935999825E-14, 0.000000000000000000 ) ) ;
#5716 = CARTESIAN_POINT ( 'NONE',  ( 14.26455149188999982, -6.229792639309999380, -9.077012475588000839 ) ) ;
#5717 = DIRECTION ( 'NONE',  ( 1.000000000000000000, 0.000000000000000000, 0.000000000000000000 ) ) ;
#5718 = CARTESIAN_POINT ( 'NONE',  ( 2.445091418594000032, 26.40256359724000035, -0.3381971108622000011 ) ) ;
#5719 = EDGE_CURVE ( 'NONE', #1386, #23264, #20163, .T. ) ;
#5720 = ORIENTED_EDGE ( 'NONE', *, *, #14420, .T. ) ;
#5721 = EDGE_LOOP ( 'NONE', ( #12838, #7284, #1616, #18568 ) ) ;
#5722 = EDGE_CURVE ( 'NONE', #15990, #23046, #23831, .T. ) ;
#5723 = CARTESIAN_POINT ( 'NONE',  ( -10.91261613876999981, -1.790000681266999960, -15.11279232617999924 ) ) ;
#5724 = CARTESIAN_POINT ( 'NONE',  ( 4.835177208035999818, -12.44999999999999929, 0.000000000000000000 ) ) ;
#5725 = CARTESIAN_POINT ( 'NONE',  ( -24.41513307467231186, -9.801374016731797312, -8.023466425255969980 ) ) ;
#5726 = ORIENTED_EDGE ( 'NONE', *, *, #6268, .T. ) ;
#5727 = CARTESIAN_POINT ( 'NONE',  ( -24.50000000000294165, 10.56908696370082446, 6.693804389267354438 ) ) ;
#5728 = CARTESIAN_POINT ( 'NONE',  ( 19.32313885814015819, -10.19623967642864670, -2.501916320087661738 ) ) ;
#5729 = LINE ( 'NONE', #10950, #19579 ) ;
#5730 = CARTESIAN_POINT ( 'NONE',  ( 16.15164999724400730, -4.403807630409194651, -9.396662404489285692 ) ) ;
#5731 = CIRCLE ( 'NONE', #6116, 0.1000000000000003525 ) ;
#5732 = CARTESIAN_POINT ( 'NONE',  ( -19.28206573533999801, -9.640750581229999838, -5.573920775363999880 ) ) ;
#5733 = CARTESIAN_POINT ( 'NONE',  ( 1.542578681836999976, 28.93232406860999717, 1.552159782388999876 ) ) ;
#5734 = CARTESIAN_POINT ( 'NONE',  ( -12.99567423753000028, 6.199143636224999199, -8.762012042742998830 ) ) ;
#5735 = STYLED_ITEM ( 'NONE', ( #16892 ), #8659 ) ;
#5736 = CARTESIAN_POINT ( 'NONE',  ( 0.2039437053001954547, 29.61575808220096206, 2.150321007061429146 ) ) ;
#5737 = EDGE_LOOP ( 'NONE', ( #10070, #11047, #20859, #21558 ) ) ;
#5738 = CARTESIAN_POINT ( 'NONE',  ( -0.2525366025761000000, 25.24749154463999901, -2.166821629601999977 ) ) ;
#5739 = CARTESIAN_POINT ( 'NONE',  ( 22.31375937178523117, 9.342772961303669632, 4.957017412827640079 ) ) ;
#5740 = DIRECTION ( 'NONE',  ( 0.000000000000000000, -0.9761919106981273853, 0.2169086293524060682 ) ) ;
#5741 = AXIS2_PLACEMENT_3D ( 'NONE', #11569, #6097, #9744 ) ;
#5742 = ORIENTED_EDGE ( 'NONE', *, *, #9402, .T. ) ;
#5743 = CARTESIAN_POINT ( 'NONE',  ( -5.366767308139002601, 16.51611458662000942, 3.205250738674000566 ) ) ;
#5744 = DIRECTION ( 'NONE',  ( 0.000000000000000000, 1.000000000000000000, 0.000000000000000000 ) ) ;
#5745 = CARTESIAN_POINT ( 'NONE',  ( 11.83106375730999993, 2.025755645688000151, -8.855592440447001223 ) ) ;
#5746 = VERTEX_POINT ( 'NONE', #16681 ) ;
#5747 = CARTESIAN_POINT ( 'NONE',  ( -4.619909110842619349, 15.59001540809187780, 4.021459351379646385 ) ) ;
#5748 = CARTESIAN_POINT ( 'NONE',  ( -14.47158022755351325, 2.069973096334361884, -12.49996948346235470 ) ) ;
#5749 = AXIS2_PLACEMENT_3D ( 'NONE', #11404, #4123, #8129 ) ;
#5750 = ORIENTED_EDGE ( 'NONE', *, *, #13248, .F. ) ;
#5751 = CARTESIAN_POINT ( 'NONE',  ( -23.08127083529245027, 7.060724976932586827, -6.230165419677522465 ) ) ;
#5752 = CARTESIAN_POINT ( 'NONE',  ( -4.622166446016002794, 12.56867761721000676, 1.067424028279999826 ) ) ;
#5753 = CONICAL_SURFACE ( 'NONE', #13476, 2.249999993279999888, 0.7853981633972997312 ) ;
#5754 = COLOUR_RGB ( '', 0.09019608, 0.27058824, 0.51372549) ;
#5755 = B_SPLINE_CURVE_WITH_KNOTS ( 'NONE', 3,
 ( #11098, #13262, #20653, #18482, #1895, #4064, #11458, #16659, #18833, #2239, #63, #6480, #4547, #10116 ),
 .UNSPECIFIED., .F., .F.,
 ( 4, 2, 2, 2, 2, 2, 4 ),
 ( 0.0001520356277385664402, 0.001067258118390845053, 0.001982480609043124099, 0.002440091854369263839, 0.002897703099695404013, 0.003355314345021543319, 0.003812925590347683059 ),
 .UNSPECIFIED. ) ;
#5756 = CARTESIAN_POINT ( 'NONE',  ( 12.00000000000000000, 1.135109584198050303, -9.208780385958741377 ) ) ;
#5757 = PRODUCT_DEFINITION ( 'UNKNOWN', '', #16751, #1998 ) ;
#5758 = LINE ( 'NONE', #13496, #17267 ) ;
#5759 = CLOSED_SHELL ( 'NONE', ( #23018, #16518, #20058, #1427, #7554, #9242, #8346 ) ) ;
#5760 = CARTESIAN_POINT ( 'NONE',  ( -5.155920576390994547, 15.83913996291999204, -2.700030400707001288 ) ) ;
#5761 = CARTESIAN_POINT ( 'NONE',  ( 2.500000000000000000, 26.80000000000000071, 0.000000000000000000 ) ) ;
#5762 = AXIS2_PLACEMENT_3D ( 'NONE', #3746, #102, #7487 ) ;
#5763 = CARTESIAN_POINT ( 'NONE',  ( 5.299443700753212028, 13.76429532417504831, -4.351754427252301660 ) ) ;
#5764 = CARTESIAN_POINT ( 'NONE',  ( 1.999167105995449445, 27.91753006952333749, -1.536366799937288530 ) ) ;
#5765 = CARTESIAN_POINT ( 'NONE',  ( 1.380771013157804372, 30.49197061622366078, 1.664552687405546960 ) ) ;
#5766 = ORIENTED_EDGE ( 'NONE', *, *, #22866, .T. ) ;
#5767 = CYLINDRICAL_SURFACE ( 'NONE', #6154, 1.500000000000000222 ) ;
#5768 = CARTESIAN_POINT ( 'NONE',  ( 14.86901153711125012, -8.273827554593831124, 3.800866100364200584 ) ) ;
#5769 = CARTESIAN_POINT ( 'NONE',  ( -23.57552075937401526, -7.930447722602094629, -5.012726446680143333 ) ) ;
#5770 = AXIS2_PLACEMENT_3D ( 'NONE', #6708, #21371, #4788 ) ;
#5771 = CARTESIAN_POINT ( 'NONE',  ( -23.24158279258278625, -3.596034818408476053, 9.948339823417249761 ) ) ;
#5772 = CARTESIAN_POINT ( 'NONE',  ( -0.2246974795679000103, 26.60114211381999993, -2.281391790424999844 ) ) ;
#5773 = CARTESIAN_POINT ( 'NONE',  ( -2.121106334292000017, 30.87889366360999688, 6.284935476095000148E-07 ) ) ;
#5774 = CARTESIAN_POINT ( 'NONE',  ( -6.414809095751526691, 26.44559118008276144, 1.018491744841189872 ) ) ;
#5775 = VERTEX_POINT ( 'NONE', #16214 ) ;
#5776 = CARTESIAN_POINT ( 'NONE',  ( -2.752375951156815326, 11.80288882812367390, -3.961635973783927511 ) ) ;
#5777 = CARTESIAN_POINT ( 'NONE',  ( 23.99062354302999722, -13.93375672974000068, -0.8660254037843999608 ) ) ;
#5778 = VECTOR ( 'NONE', #15171, 1000.000000000000000 ) ;
#5779 = CARTESIAN_POINT ( 'NONE',  ( -21.35476253787999923, 9.219287007783998789, 0.000000000000000000 ) ) ;
#5780 = ORIENTED_EDGE ( 'NONE', *, *, #514, .T. ) ;
#5781 = DIRECTION ( 'NONE',  ( 1.000000000000000000, 0.000000000000000000, 0.000000000000000000 ) ) ;
#5782 = CARTESIAN_POINT ( 'NONE',  ( 14.95518908531000157, 0.8306535110907999897, 10.15076156001000207 ) ) ;
#5783 = EDGE_CURVE ( 'NONE', #16380, #20998, #15100, .T. ) ;
#5784 = CARTESIAN_POINT ( 'NONE',  ( -19.82722067471999949, -8.836429628019001115, 5.355976217871000422 ) ) ;
#5785 = FACE_OUTER_BOUND ( 'NONE', #22347, .T. ) ;
#5786 = CARTESIAN_POINT ( 'NONE',  ( 17.76551537305999773, -10.38510595533999847, 3.229171968965000250 ) ) ;
#5787 = CARTESIAN_POINT ( 'NONE',  ( 0.1526552725783049125, 24.50000000000000000, 2.395140156181688074 ) ) ;
#5788 = VERTEX_POINT ( 'NONE', #7241 ) ;
#5789 = FACE_OUTER_BOUND ( 'NONE', #8706, .T. ) ;
#5790 = CARTESIAN_POINT ( 'NONE',  ( 21.28115130527999810, -8.293037263826001038, 6.853370783829999091 ) ) ;
#5791 = LINE ( 'NONE', #17165, #23922 ) ;
#5792 = ORIENTED_EDGE ( 'NONE', *, *, #21364, .F. ) ;
#5793 = CARTESIAN_POINT ( 'NONE',  ( 11.38563810340999893, -8.030754667131001057, -4.228659338699999104 ) ) ;
#5794 = DIRECTION ( 'NONE',  ( 0.000000000000000000, 1.000000000000000000, 0.000000000000000000 ) ) ;
#5795 = AXIS2_PLACEMENT_3D ( 'NONE', #23832, #23956, #16215 ) ;
#5796 = CARTESIAN_POINT ( 'NONE',  ( 4.835175158044003219, 12.42241705055999823, 0.2482835134780999597 ) ) ;
#5797 = CARTESIAN_POINT ( 'NONE',  ( -0.9120910450028335559, 29.25920337588331321, -1.958506303686876393 ) ) ;
#5798 = EDGE_CURVE ( 'NONE', #4163, #15215, #23611, .T. ) ;
#5799 = CARTESIAN_POINT ( 'NONE',  ( -19.19184533664999748, -10.45696971737000069, 1.867641980438999871 ) ) ;
#5800 = ORIENTED_EDGE ( 'NONE', *, *, #6277, .T. ) ;
#5801 = PLANE ( 'NONE',  #9978 ) ;
#5802 = ORIENTED_EDGE ( 'NONE', *, *, #16764, .F. ) ;
#5803 = CARTESIAN_POINT ( 'NONE',  ( 0.5680559541153000769, 25.57756168797000029, 2.085265971965999832 ) ) ;
#5804 = CARTESIAN_POINT ( 'NONE',  ( -2.434931691670787934, 28.03333333333334210, 0.6543697108982051702 ) ) ;
#5805 = CARTESIAN_POINT ( 'NONE',  ( -2.263084017374999757, 26.89799822780999961, 0.1334610483750000021 ) ) ;
#5806 = CARTESIAN_POINT ( 'NONE',  ( 6.243179582884000212, 1.578914512950999657E-14, -13.77250448649344250 ) ) ;
#5807 = CARTESIAN_POINT ( 'NONE',  ( -12.50000000000000000, 1.557342902441000195E-14, 1.045589212608000028E-14 ) ) ;
#5808 = DIRECTION ( 'NONE',  ( -0.000000000000000000, -0.000000000000000000, 1.000000000000000000 ) ) ;
#5809 = CARTESIAN_POINT ( 'NONE',  ( 14.98162674931000105, 7.974294229383000143, 7.126218918095000632 ) ) ;
#5810 = CARTESIAN_POINT ( 'NONE',  ( -14.21445632535000136, 4.821896674351999756, 9.628268207709998805 ) ) ;
#5811 = CARTESIAN_POINT ( 'NONE',  ( -2.500000000000000000, 28.80000000000000071, 0.000000000000000000 ) ) ;
#5812 = CARTESIAN_POINT ( 'NONE',  ( -14.49863740500227038, -0.5184489068381992194, 12.49996363569670521 ) ) ;
#5813 = ADVANCED_FACE ( 'NONE', ( #3399 ), #8893, .F. ) ;
#5814 = ORIENTED_EDGE ( 'NONE', *, *, #13218, .T. ) ;
#5815 = CARTESIAN_POINT ( 'NONE',  ( -10.62523811313343991, 15.45380396666532263, -1.485942923904584489 ) ) ;
#5816 = CARTESIAN_POINT ( 'NONE',  ( 2.305541151813000234, 24.64511087984000071, -1.435767851291000152 ) ) ;
#5817 = CARTESIAN_POINT ( 'NONE',  ( 13.84556716760639006, -8.683927038290656597, 5.545870859834080235 ) ) ;
#5818 = DIRECTION ( 'NONE',  ( 0.000000000000000000, 1.000000000000000000, 0.000000000000000000 ) ) ;
#5819 = CARTESIAN_POINT ( 'NONE',  ( 19.83046186496999752, -1.917974774180999820, -11.02115077512000063 ) ) ;
#5820 = CARTESIAN_POINT ( 'NONE',  ( 2.435082195634000080, 29.44076328160999978, 0.7672906025640999772 ) ) ;
#5821 = CARTESIAN_POINT ( 'NONE',  ( 13.76087388038597936, 8.957244340564407992, -1.248995784414053345 ) ) ;
#5822 = LINE ( 'NONE', #20597, #14636 ) ;
#5823 = DIRECTION ( 'NONE',  ( 0.000000000000000000, 0.000000000000000000, -1.000000000000000000 ) ) ;
#5824 = ADVANCED_FACE ( 'NONE', ( #14746 ), #2796, .F. ) ;
#5825 = CARTESIAN_POINT ( 'NONE',  ( 11.90008533511768896, 13.14613689767754146, -2.230302227733069298 ) ) ;
#5826 = VERTEX_POINT ( 'NONE', #14258 ) ;
#5827 = CARTESIAN_POINT ( 'NONE',  ( 24.25008227645999881, 0.000000000000000000, 0.000000000000000000 ) ) ;
#5828 = CARTESIAN_POINT ( 'NONE',  ( 1.792728101376139804, 23.95620205949097326, -1.699880397723725789 ) ) ;
#5829 = ORIENTED_EDGE ( 'NONE', *, *, #6087, .T. ) ;
#5830 = DIRECTION ( 'NONE',  ( -1.000000000000000000, 0.000000000000000000, 0.000000000000000000 ) ) ;
#5831 = DIRECTION ( 'NONE',  ( 1.000000000000000000, 0.000000000000000000, 0.000000000000000000 ) ) ;
#5832 = CARTESIAN_POINT ( 'NONE',  ( 13.36229700266000187, 5.683036826372999784, 8.581013501291998580 ) ) ;
#5833 = AXIS2_PLACEMENT_3D ( 'NONE', #2494, #2255, #9764 ) ;
#5834 = CARTESIAN_POINT ( 'NONE',  ( -12.41173981160000039, 6.613190111079999767, -13.46349570337000046 ) ) ;
#5835 = CARTESIAN_POINT ( 'NONE',  ( 1.687576972922000040, 27.65419433610000155, 2.322750540216000026 ) ) ;
#5836 = ORIENTED_EDGE ( 'NONE', *, *, #10757, .F. ) ;
#5837 = ORIENTED_EDGE ( 'NONE', *, *, #9282, .F. ) ;
#5838 = CARTESIAN_POINT ( 'NONE',  ( -14.00000000000000178, -9.062199998400112477, -4.448848724211252659 ) ) ;
#5839 = CARTESIAN_POINT ( 'NONE',  ( -11.92346721169000112, 5.896127864781000483, 14.40918513707999971 ) ) ;
#5840 = DIRECTION ( 'NONE',  ( 0.000000000000000000, -1.000000000000000000, 0.000000000000000000 ) ) ;
#5841 = CARTESIAN_POINT ( 'NONE',  ( -24.27585716846449060, -9.160327548061168557, -9.133709619347802899 ) ) ;
#5842 = EDGE_CURVE ( 'NONE', #13740, #6468, #1655, .T. ) ;
#5843 = ORIENTED_EDGE ( 'NONE', *, *, #19473, .F. ) ;
#5844 = EDGE_CURVE ( 'NONE', #16663, #13012, #23573, .T. ) ;
#5845 = CARTESIAN_POINT ( 'NONE',  ( 20.08416666666666828, -9.000201972419345609, 2.126478957478491694 ) ) ;
#5846 = CARTESIAN_POINT ( 'NONE',  ( 19.52904096179855031, -6.069165301658948408, -8.568664490119912713 ) ) ;
#5847 = DIRECTION ( 'NONE',  ( 1.000000000000000000, 0.000000000000000000, 0.000000000000000000 ) ) ;
#5848 = CARTESIAN_POINT ( 'NONE',  ( 15.56286596738189942, -6.410929410329065270, 8.147947015818964189 ) ) ;
#5849 = CARTESIAN_POINT ( 'NONE',  ( -14.98018789272999918, 7.746190468795000506, -7.835402896861000777 ) ) ;
#5850 = CARTESIAN_POINT ( 'NONE',  ( 2.111381028812000515, 29.62342848812999918, -0.5916485676189999765 ) ) ;
#5851 = CARTESIAN_POINT ( 'NONE',  ( -14.62071702128999995, 10.29594144910999809, -3.192455093500000007 ) ) ;
#5852 = CARTESIAN_POINT ( 'NONE',  ( 1.089341972983306261, 29.67115983959759618, 1.865512284885492145 ) ) ;
#5853 = EDGE_CURVE ( 'NONE', #1942, #21964, #15730, .T. ) ;
#5854 = ORIENTED_EDGE ( 'NONE', *, *, #23442, .F. ) ;
#5855 = CARTESIAN_POINT ( 'NONE',  ( 1.153787575258000020, 24.88016091445000200, 2.030811482765999987 ) ) ;
#5856 = EDGE_CURVE ( 'NONE', #8899, #2380, #13900, .T. ) ;
#5857 = CARTESIAN_POINT ( 'NONE',  ( -4.820914651057999656, 13.20110358116999905, -5.836454220812999694 ) ) ;
#5858 = CARTESIAN_POINT ( 'NONE',  ( 4.821047785747002656, 14.92830715209997905, -3.789723698138999897 ) ) ;
#5859 = ORIENTED_EDGE ( 'NONE', *, *, #16643, .F. ) ;
#5860 = CARTESIAN_POINT ( 'NONE',  ( -2.100000000000000089, 28.30000000000000071, 0.000000000000000000 ) ) ;
#5861 = CARTESIAN_POINT ( 'NONE',  ( -4.419368126936999097, 15.75034981608000351, 4.320386041415997802 ) ) ;
#5862 = CARTESIAN_POINT ( 'NONE',  ( -6.250000000000000000, -15.43375672974000068, 0.000000000000000000 ) ) ;
#5863 = CARTESIAN_POINT ( 'NONE',  ( 12.05043875730999936, 7.573215573255999367, -5.027566056405999184 ) ) ;
#5864 = ORIENTED_EDGE ( 'NONE', *, *, #21648, .T. ) ;
#5865 = CARTESIAN_POINT ( 'NONE',  ( -6.316928638995997325, 15.85590696878002603, -1.061654000538000409 ) ) ;
#5866 = DIRECTION ( 'NONE',  ( -1.000000000000000000, 0.000000000000000000, 0.000000000000000000 ) ) ;
#5867 = AXIS2_PLACEMENT_3D ( 'NONE', #9745, #6098, #2354 ) ;
#5868 = VERTEX_POINT ( 'NONE', #20421 ) ;
#5869 = LINE ( 'NONE', #10653, #1111 ) ;
#5870 = CARTESIAN_POINT ( 'NONE',  ( -18.99854661335000117, 6.966878364870000340, -12.06698729810999993 ) ) ;
#5871 = CARTESIAN_POINT ( 'NONE',  ( -4.522737060985000390, 12.53062717673999593, 1.434513612155000395 ) ) ;
#5872 = CARTESIAN_POINT ( 'NONE',  ( -22.93944013947999849, 9.633115978054998862, -0.2991401492583000143 ) ) ;
#5873 = CARTESIAN_POINT ( 'NONE',  ( 19.22595603379665619, 4.615378250370806512, -8.008001678105078014 ) ) ;
#5874 = CARTESIAN_POINT ( 'NONE',  ( -5.340888267555999214, 16.50102740467002249, -3.245487968687000624 ) ) ;
#5875 = CARTESIAN_POINT ( 'NONE',  ( 6.243179582884000212, -13.77250448648999814, 0.000000000000000000 ) ) ;
#5876 = CIRCLE ( 'NONE', #15147, 1.500000000000000000 ) ;
#5877 = CARTESIAN_POINT ( 'NONE',  ( 0.1784790855350541494, 26.24995697614779644, -4.515757205439222766 ) ) ;
#5878 = CARTESIAN_POINT ( 'NONE',  ( 0.000000000000000000, 0.000000000000000000, 0.000000000000000000 ) ) ;
#5879 = CARTESIAN_POINT ( 'NONE',  ( -1.015987791502897419, 30.34136096126319515, 1.906676889270033426 ) ) ;
#5880 = ORIENTED_EDGE ( 'NONE', *, *, #11499, .F. ) ;
#5881 = CARTESIAN_POINT ( 'NONE',  ( 24.16831550194999778, -8.024295071342999464, -4.916962988213999353 ) ) ;
#5882 = CARTESIAN_POINT ( 'NONE',  ( 4.312196806323354004, 13.42372324865281641, -5.304433147621987921 ) ) ;
#5883 = CARTESIAN_POINT ( 'NONE',  ( 1.839173991642404582, 30.00000000000000711, 3.556954554355652220 ) ) ;
#5884 = CARTESIAN_POINT ( 'NONE',  ( -24.15197954327974372, 3.481455606802188019, -10.01183836013010442 ) ) ;
#5885 = CARTESIAN_POINT ( 'NONE',  ( 2.093446882794999908, 25.56114211382000079, 0.4710401059125000067 ) ) ;
#5886 = CARTESIAN_POINT ( 'NONE',  ( 12.00000000000000000, 0.000000000000000000, 0.000000000000000000 ) ) ;
#5887 = ORIENTED_EDGE ( 'NONE', *, *, #7018, .F. ) ;
#5888 = FACE_OUTER_BOUND ( 'NONE', #10189, .T. ) ;
#5889 = CARTESIAN_POINT ( 'NONE',  ( -4.000000000000000000, 29.69999999999999929, 2.309401076759000304 ) ) ;
#5890 = CARTESIAN_POINT ( 'NONE',  ( -4.000000000000000000, 26.20000000000000284, -2.309401076759000304 ) ) ;
#5891 = DIRECTION ( 'NONE',  ( 0.000000000000000000, -1.000000000000000000, 0.000000000000000000 ) ) ;
#5892 = DIRECTION ( 'NONE',  ( 0.000000000000000000, 1.000000000000000000, 0.000000000000000000 ) ) ;
#5893 = CARTESIAN_POINT ( 'NONE',  ( 15.72300158530999958, -5.453124986814999353, -8.625711720232999369 ) ) ;
#5894 = CARTESIAN_POINT ( 'NONE',  ( -19.62575000533999869, -7.533253386014000519, 7.382837537152000529 ) ) ;
#5895 = CARTESIAN_POINT ( 'NONE',  ( -10.04281598261999875, 16.38798294975000047, 0.9999999999983999466 ) ) ;
#5896 = CARTESIAN_POINT ( 'NONE',  ( 18.37489037306000128, 2.572692777010999965, -10.58437343029000033 ) ) ;
#5897 = CARTESIAN_POINT ( 'NONE',  ( -2.121106334292000017, 30.87889366360999688, 6.284935476095000148E-07 ) ) ;
#5898 = CONICAL_SURFACE ( 'NONE', #16736, 4.309401076758999416, 1.119376321708719590 ) ;
#5899 = FACE_OUTER_BOUND ( 'NONE', #17336, .T. ) ;
#5900 = CARTESIAN_POINT ( 'NONE',  ( 19.78196485594000009, -8.739116552734000010, 5.237636975568999986 ) ) ;
#5901 = CARTESIAN_POINT ( 'NONE',  ( 0.000000000000000000, 22.00000000000000000, 0.000000000000000000 ) ) ;
#5902 = ORIENTED_EDGE ( 'NONE', *, *, #6904, .F. ) ;
#5903 = CARTESIAN_POINT ( 'NONE',  ( 12.10937109324999916, -8.506090310477000926, -2.885017716830000190 ) ) ;
#5904 = CARTESIAN_POINT ( 'NONE',  ( 6.243179582884000212, 1.148189900220999940E-14, 0.000000000000000000 ) ) ;
#5905 = CARTESIAN_POINT ( 'NONE',  ( 4.599771440748003037, 12.33202429268000166, 1.513355409791999229 ) ) ;
#5906 = CARTESIAN_POINT ( 'NONE',  ( 2.154709788952736460, 28.99504473153596251, 0.1496538372950146079 ) ) ;
#5907 = CARTESIAN_POINT ( 'NONE',  ( -23.77359187212000080, 8.708980288023001393, 6.967567546233000009 ) ) ;
#5908 = ORIENTED_EDGE ( 'NONE', *, *, #15329, .T. ) ;
#5909 = B_SPLINE_CURVE_WITH_KNOTS ( 'NONE', 3,
 ( #8489, #23491, #15855, #5102, #12483, #19868, #7022, #12002, #10666, #18054, #1460, #14409, #8362, #23837, #96, #22147, #18395, #3864, #2040, #22037, #14523, #3627, #5446, #16572, #23962, #16686, #18514, #20110, #20451, #21914, #7481, #20332 ),
 .UNSPECIFIED., .F., .F.,
 ( 4, 2, 2, 2, 2, 2, 2, 2, 2, 2, 2, 2, 1, 2, 1, 2, 4 ),
 ( 0.000000000000000000, 0.06250000000000006939, 0.1250000000000001388, 0.1875000000000002220, 0.2500000000000002776, 0.3125000000000002776, 0.3750000000000002776, 0.4375000000000003331, 0.5000000000000003331, 0.5625000000000003331, 0.6250000000000002220, 0.6875000000000002220, 0.7500000000000001110, 0.8125000000000001110, 0.8750000000000001110, 0.9375000000000000000, 1.000000000000000000 ),
 .UNSPECIFIED. ) ;
#5910 = CARTESIAN_POINT ( 'NONE',  ( 24.24531177150999994, 0.000000000000000000, 0.000000000000000000 ) ) ;
#5911 = ORIENTED_EDGE ( 'NONE', *, *, #12035, .T. ) ;
#5912 = EDGE_CURVE ( 'NONE', #165, #7280, #3829, .T. ) ;
#5913 = CARTESIAN_POINT ( 'NONE',  ( 15.63574770046331430, 5.575401216236696378, -7.255087836980721683 ) ) ;
#5914 = CARTESIAN_POINT ( 'NONE',  ( 0.6543697108982093891, 28.23333333333333428, 2.434931691670787046 ) ) ;
#5915 = CARTESIAN_POINT ( 'NONE',  ( 2.231710853292999897, 28.06799822781000131, 0.3985328791175999918 ) ) ;
#5916 = DIRECTION ( 'NONE',  ( 1.000000000000000000, 0.000000000000000000, 0.000000000000000000 ) ) ;
#5917 = CYLINDRICAL_SURFACE ( 'NONE', #21154, 4.724999999999999645 ) ;
#5918 = CARTESIAN_POINT ( 'NONE',  ( 16.84631424931000154, 6.637278256850999369, 8.448060240267999177 ) ) ;
#5919 = DIRECTION ( 'NONE',  ( 0.000000000000000000, 0.000000000000000000, 1.000000000000000000 ) ) ;
#5920 = CARTESIAN_POINT ( 'NONE',  ( -17.42378381163999990, -1.451785825221999948, 10.21952336923999916 ) ) ;
#5921 = CARTESIAN_POINT ( 'NONE',  ( 4.000000000000000000, 30.00000000000000000, 0.000000000000000000 ) ) ;
#5922 = AXIS2_PLACEMENT_3D ( 'NONE', #19405, #6800, #4757 ) ;
#5923 = DIRECTION ( 'NONE',  ( 0.000000000000000000, 1.000000000000000000, 0.000000000000000000 ) ) ;
#5924 = ORIENTED_EDGE ( 'NONE', *, *, #9875, .T. ) ;
#5925 = EDGE_CURVE ( 'NONE', #10616, #16623, #16889, .T. ) ;
#5926 = CARTESIAN_POINT ( 'NONE',  ( -2.127181242815999962, 23.63919896736999604, 0.9631217529048999859 ) ) ;
#5927 = CARTESIAN_POINT ( 'NONE',  ( 13.63524120837945830, -2.821342633397881272, 9.926079101813042982 ) ) ;
#5928 = CARTESIAN_POINT ( 'NONE',  ( 2.917722632763000146, 13.60402666298999996, -5.360392733824004274 ) ) ;
#5929 = CARTESIAN_POINT ( 'NONE',  ( 21.07836523965000097, -5.385920316227999827, 9.843973735277000259 ) ) ;
#5930 = CARTESIAN_POINT ( 'NONE',  ( -1.236897034087000025, 30.01523436640999876, 2.233482906277000080 ) ) ;
#5931 = CARTESIAN_POINT ( 'NONE',  ( 11.09594815121216271, -0.9954690943958549587, 12.49999871278813046 ) ) ;
#5932 = CARTESIAN_POINT ( 'NONE',  ( -6.722873803920665026, 15.34560435500414144, -1.730847659303734298 ) ) ;
#5933 = CARTESIAN_POINT ( 'NONE',  ( -6.313954834032534436, 15.63752586476230633, 1.252296258704070464 ) ) ;
#5934 = CARTESIAN_POINT ( 'NONE',  ( -1.536366799937290084, 29.71753006952332399, -1.999167105995447669 ) ) ;
#5935 = ORIENTED_EDGE ( 'NONE', *, *, #13685, .F. ) ;
#5936 = CARTESIAN_POINT ( 'NONE',  ( 1.600000000000000089, 8.900000000000000355, -1.856657105836000120E-09 ) ) ;
#5937 = ORIENTED_EDGE ( 'NONE', *, *, #18467, .F. ) ;
#5938 = EDGE_CURVE ( 'NONE', #4848, #22927, #11669, .T. ) ;
#5939 = CARTESIAN_POINT ( 'NONE',  ( 1.123018145447999938, 25.40617362301000171, -2.496154155557999577 ) ) ;
#5940 = CARTESIAN_POINT ( 'NONE',  ( 24.36165043081784276, 9.237917109185875830, 8.999458210778742639 ) ) ;
#5941 = FACE_OUTER_BOUND ( 'NONE', #18670, .T. ) ;
#5942 = ORIENTED_EDGE ( 'NONE', *, *, #1664, .F. ) ;
#5943 = CARTESIAN_POINT ( 'NONE',  ( 14.08410059404000059, -10.35854663702999900, -3.714083093220999832 ) ) ;
#5944 = CARTESIAN_POINT ( 'NONE',  ( 30.87226923053214378, 37.01856778792605240, -2.673746900119611247 ) ) ;
#5945 = CARTESIAN_POINT ( 'NONE',  ( -2.411020654974999733, 26.01256359723999978, 0.5289967318968999965 ) ) ;
#5946 = ORIENTED_EDGE ( 'NONE', *, *, #16379, .T. ) ;
#5947 = ORIENTED_EDGE ( 'NONE', *, *, #18378, .F. ) ;
#5948 = CARTESIAN_POINT ( 'NONE',  ( -24.46742986864730796, 10.18447769906778788, -7.359979596042377281 ) ) ;
#5949 = CARTESIAN_POINT ( 'NONE',  ( -2.500000000000000888, 27.41753006952333749, -0.3272492347489316944 ) ) ;
#5950 = CARTESIAN_POINT ( 'NONE',  ( 4.649999849441000421, 19.99999984944626874, -6.648422669304000250E-08 ) ) ;
#5951 = CONICAL_SURFACE ( 'NONE', #9440, 4.699999872533999756, 0.7853981633972997312 ) ;
#5952 = CARTESIAN_POINT ( 'NONE',  ( 17.88295603379667043, 7.701996700470298940, 5.081089778053197392 ) ) ;
#5953 = EDGE_LOOP ( 'NONE', ( #16932, #17799, #2200, #8525, #7704 ) ) ;
#5954 = EDGE_CURVE ( 'NONE', #11139, #12251, #17793, .T. ) ;
#5955 = CARTESIAN_POINT ( 'NONE',  ( -19.60267883610000084, 8.869063186870999260, -3.716108411551000579 ) ) ;
#5956 = CARTESIAN_POINT ( 'NONE',  ( -14.41332674684316828, 12.63239273138172436, 3.119888754832823796 ) ) ;
#5957 = CARTESIAN_POINT ( 'NONE',  ( 6.225676751962361699, 13.76137232892522633, 1.306414714001897126 ) ) ;
#5958 = CARTESIAN_POINT ( 'NONE',  ( 15.73262886950022654, -9.839481850775154470, 3.264375423814056987 ) ) ;
#5959 = CARTESIAN_POINT ( 'NONE',  ( -15.19489292590999874, -5.010861156605001199, -9.819261828225998912 ) ) ;
#5960 = CARTESIAN_POINT ( 'NONE',  ( -1.799241820176000095, 29.91117657083000125, -1.253278400384999935 ) ) ;
#5961 = VECTOR ( 'NONE', #6528, 1000.000000000000000 ) ;
#5962 = CARTESIAN_POINT ( 'NONE',  ( -17.91156067002999919, -1.604197317876000062, 11.29338059605000133 ) ) ;
#5963 = ADVANCED_FACE ( 'NONE', ( #10334 ), #22402, .F. ) ;
#5964 = CARTESIAN_POINT ( 'NONE',  ( -0.06398334756564613701, 29.60010643587459711, 2.158911828703185432 ) ) ;
#5965 = ORIENTED_EDGE ( 'NONE', *, *, #5292, .T. ) ;
#5966 = CARTESIAN_POINT ( 'NONE',  ( -2.335877486882000031, 24.40855709534999818, -0.2468828260556999998 ) ) ;
#5967 = AXIS2_PLACEMENT_3D ( 'NONE', #17722, #14328, #1120 ) ;
#5968 = CARTESIAN_POINT ( 'NONE',  ( -18.57237735687682445, 10.43290785388021291, -0.7825199175144633701 ) ) ;
#5969 = ORIENTED_EDGE ( 'NONE', *, *, #10158, .F. ) ;
#5970 = ADVANCED_FACE ( 'NONE', ( #14202 ), #20873, .T. ) ;
#5971 = CARTESIAN_POINT ( 'NONE',  ( -4.858535779299999469, 13.29855084970999890, 5.919202098683998159 ) ) ;
#5972 = EDGE_CURVE ( 'NONE', #4443, #10646, #10448, .T. ) ;
#5973 = AXIS2_PLACEMENT_3D ( 'NONE', #998, #23031, #6689 ) ;
#5974 = CARTESIAN_POINT ( 'NONE',  ( -14.00000000000000178, -10.31294900121941005, -0.06607431037178398969 ) ) ;
#5975 = CARTESIAN_POINT ( 'NONE',  ( 18.51187642130999933, -4.805399430337999434, 8.325799818148999165 ) ) ;
#5976 = ORIENTED_EDGE ( 'NONE', *, *, #8212, .F. ) ;
#5977 = CARTESIAN_POINT ( 'NONE',  ( -130.2348000000000070, 19.50000000000000000, -5.000000000000000000 ) ) ;
#5978 = DIRECTION ( 'NONE',  ( -0.7071067811865969777, -0.7071067811864980568, -2.474840881013989736E-09 ) ) ;
#5979 = ORIENTED_EDGE ( 'NONE', *, *, #17236, .T. ) ;
#5980 = EDGE_CURVE ( 'NONE', #8904, #14691, #21719, .T. ) ;
#5981 = CARTESIAN_POINT ( 'NONE',  ( -16.55522087121331865, -5.589901749525623131, -7.273956370960904749 ) ) ;
#5982 = CARTESIAN_POINT ( 'NONE',  ( 21.81383333333333141, -8.065932698539254986, 4.649058171626129443 ) ) ;
#5983 = CARTESIAN_POINT ( 'NONE',  ( 4.414629580919998020, 12.49396588617999271, 1.935277879409999624 ) ) ;
#5984 = VECTOR ( 'NONE', #14406, 1000.000000000000000 ) ;
#5985 = CARTESIAN_POINT ( 'NONE',  ( 23.41677564524290744, 34.01856778792605240, -6.000000000000000000 ) ) ;
#5986 = CARTESIAN_POINT ( 'NONE',  ( -21.97592002967000013, -9.481613672941000104, -1.576156473507000166 ) ) ;
#5987 = DIRECTION ( 'NONE',  ( 1.000000000000000000, 0.000000000000000000, 0.000000000000000000 ) ) ;
#5988 = CARTESIAN_POINT ( 'NONE',  ( -11.99999999434999864, -6.999999994347000154, -4.083277946868999946E-09 ) ) ;
#5989 = CARTESIAN_POINT ( 'NONE',  ( -12.50000000000000000, 6.992973968623999781, -5.709239639804999378 ) ) ;
#5990 = CARTESIAN_POINT ( 'NONE',  ( 5.562517841236772398, 14.53154872498324579, 2.570889057986909698 ) ) ;
#5991 = CARTESIAN_POINT ( 'NONE',  ( 1.709999999999999964, 0.000000000000000000, 0.000000000000000000 ) ) ;
#5992 = CARTESIAN_POINT ( 'NONE',  ( 0.5486518589655812184, 30.43653985558582420, 2.089137083840504783 ) ) ;
#5993 = ORIENTED_EDGE ( 'NONE', *, *, #22539, .F. ) ;
#5994 = CARTESIAN_POINT ( 'NONE',  ( 22.68672501132000008, 1.244886420992999954, -9.776971065933000915 ) ) ;
#5995 = CARTESIAN_POINT ( 'NONE',  ( -2.218324364786688818, 12.96888396011062738, -6.336184367259724226 ) ) ;
#5996 = DIRECTION ( 'NONE',  ( 0.000000000000000000, 1.000000000000000000, 0.000000000000000000 ) ) ;
#5997 = EDGE_CURVE ( 'NONE', #13163, #20695, #13126, .T. ) ;
#5998 = CARTESIAN_POINT ( 'NONE',  ( -21.01914366587545402, -10.32835885544590582, -1.990128420184432700 ) ) ;
#5999 = FACE_OUTER_BOUND ( 'NONE', #19790, .T. ) ;
#6000 = ADVANCED_FACE ( 'NONE', ( #12151 ), #12754, .F. ) ;
#6001 = AXIS2_PLACEMENT_3D ( 'NONE', #1923, #12713, #7245 ) ;
#6002 = CARTESIAN_POINT ( 'NONE',  ( -0.6838519464012248195, 28.13336607546796841, 4.223839491855484241 ) ) ;
#6003 = VERTEX_POINT ( 'NONE', #1243 ) ;
#6004 = CARTESIAN_POINT ( 'NONE',  ( 2.750000000000000000, 22.19999999999999574, 0.000000000000000000 ) ) ;
#6005 = LINE ( 'NONE', #5777, #15745 ) ;
#6006 = CARTESIAN_POINT ( 'NONE',  ( 2.053005267516999902E-14, 28.63049582772000079, 2.160000000000000142 ) ) ;
#6007 = APPLICATION_CONTEXT ( 'automotive_design' ) ;
#6008 = VERTEX_POINT ( 'NONE', #17963 ) ;
#6009 = ORIENTED_EDGE ( 'NONE', *, *, #6285, .T. ) ;
#6010 = EDGE_CURVE ( 'NONE', #2558, #15509, #19214, .T. ) ;
#6011 = DIRECTION ( 'NONE',  ( 0.000000000000000000, 0.000000000000000000, -1.000000000000000000 ) ) ;
#6012 = CARTESIAN_POINT ( 'NONE',  ( 13.99443924931000005, -9.599271117524001085, -4.655318192544999789 ) ) ;
#6013 = CIRCLE ( 'NONE', #15288, 0.5500000000000001554 ) ;
#6014 = CARTESIAN_POINT ( 'NONE',  ( -14.75062165406000148, 10.41229764572999983, 4.438028563735000098 ) ) ;
#6015 = CARTESIAN_POINT ( 'NONE',  ( 0.000000000000000000, 28.00000000000000000, 0.000000000000000000 ) ) ;
#6016 = CARTESIAN_POINT ( 'NONE',  ( 15.32801537305999950, 8.400340696411999986, 6.799953174600000594 ) ) ;
#6017 = DIRECTION ( 'NONE',  ( 0.000000000000000000, 0.000000000000000000, -1.000000000000000000 ) ) ;
#6018 = DIRECTION ( 'NONE',  ( 0.000000000000000000, 0.000000000000000000, -1.000000000000000000 ) ) ;
#6019 = CARTESIAN_POINT ( 'NONE',  ( 23.77130057337999958, -9.515117350267999541, 2.208807626390000056 ) ) ;
#6020 = DIRECTION ( 'NONE',  ( -0.9996708941621511579, -0.02565352539213875543, -5.387480945348741403E-14 ) ) ;
#6021 = VERTEX_POINT ( 'NONE', #13677 ) ;
#6022 = CARTESIAN_POINT ( 'NONE',  ( 11.99054877623999893, -6.470940098446000377, -6.715655461047000507 ) ) ;
#6023 = CARTESIAN_POINT ( 'NONE',  ( 2.159851832628000068, 26.67456776951999942, 1.569224139466999901 ) ) ;
#6024 = CARTESIAN_POINT ( 'NONE',  ( -0.1178155359250000339, 11.45056912575998886, 4.946867145734003657 ) ) ;
#6025 = CARTESIAN_POINT ( 'NONE',  ( 24.50000000000000000, -9.344098705406999272, -3.489386534399999906 ) ) ;
#6026 = CARTESIAN_POINT ( 'NONE',  ( -23.79405482100999691, 11.10233715562999990, 1.069494977660000012 ) ) ;
#6027 = ORIENTED_EDGE ( 'NONE', *, *, #23448, .T. ) ;
#6028 = DIRECTION ( 'NONE',  ( 0.000000000000000000, 1.000000000000000000, 0.000000000000000000 ) ) ;
#6029 = ORIENTED_EDGE ( 'NONE', *, *, #6558, .T. ) ;
#6030 = CARTESIAN_POINT ( 'NONE',  ( 3.792292039899240574, 12.19805237062407954, 2.925708645425909804 ) ) ;
#6031 = CARTESIAN_POINT ( 'NONE',  ( -1.978081431919000099, 28.55549822781000202, 1.107772814030999919 ) ) ;
#6032 = CARTESIAN_POINT ( 'NONE',  ( -4.752065375082999310, 13.48440873408998364, 5.196329956053004295 ) ) ;
#6033 = AXIS2_PLACEMENT_3D ( 'NONE', #8136, #13572, #22768 ) ;
#6034 = VECTOR ( 'NONE', #6323, 1000.000000000000114 ) ;
#6035 = CARTESIAN_POINT ( 'NONE',  ( 0.000000000000000000, 13.04999996922999905, -4.674999969225999585 ) ) ;
#6036 = CARTESIAN_POINT ( 'NONE',  ( 16.07850174930999998, -1.960161522604999762, -10.54265994730999978 ) ) ;
#6037 = CARTESIAN_POINT ( 'NONE',  ( -16.85515084895999749, -2.006433207287000364, -10.65451757797000099 ) ) ;
#6038 = CARTESIAN_POINT ( 'NONE',  ( 14.35387625730999872, 4.075369344914999914, 8.193037116081999471 ) ) ;
#6039 = CARTESIAN_POINT ( 'NONE',  ( 24.34804274388857337, 12.49056186101158872, -3.365712241645715253 ) ) ;
#6040 = ORIENTED_EDGE ( 'NONE', *, *, #5997, .T. ) ;
#6041 = AXIS2_PLACEMENT_3D ( 'NONE', #17386, #9997, #2362 ) ;
#6042 = CARTESIAN_POINT ( 'NONE',  ( -1.836544194422999876, 24.06874085023000021, -2.001013430241999735 ) ) ;
#6043 = CARTESIAN_POINT ( 'NONE',  ( 13.65222839007885192, -3.408405854262552381, 9.739428946578977175 ) ) ;
#6044 = FACE_OUTER_BOUND ( 'NONE', #3941, .T. ) ;
#6045 = CARTESIAN_POINT ( 'NONE',  ( 19.97708346185000039, -1.918664432208000203, -11.02511595671000144 ) ) ;
#6046 = EDGE_CURVE ( 'NONE', #22071, #9831, #119, .T. ) ;
#6047 = CARTESIAN_POINT ( 'NONE',  ( -0.8128465029875000525, 30.41246193502999873, -2.622577599952000238 ) ) ;
#6048 = CARTESIAN_POINT ( 'NONE',  ( 14.46013925473697981, -5.946942342394209824, 6.857621950180825543 ) ) ;
#6049 = CARTESIAN_POINT ( 'NONE',  ( 18.23920040721611358, 9.753634886311211005, -3.797171640280522897 ) ) ;
#6050 = CARTESIAN_POINT ( 'NONE',  ( 0.000000000000000000, 13.10000000000000142, 0.000000000000000000 ) ) ;
#6051 = LINE ( 'NONE', #3777, #9856 ) ;
#6052 = CARTESIAN_POINT ( 'NONE',  ( 24.37713355803437665, -12.31988888405492411, -3.661326509212557756 ) ) ;
#6053 = ORIENTED_EDGE ( 'NONE', *, *, #8147, .F. ) ;
#6054 = DIRECTION ( 'NONE',  ( 0.000000000000000000, -1.000000000000000000, 0.000000000000000000 ) ) ;
#6055 = VERTEX_POINT ( 'NONE', #4362 ) ;
#6056 = CARTESIAN_POINT ( 'NONE',  ( -5.778907386873838092, 16.26325521095871451, -2.029774016053516927 ) ) ;
#6058 = CARTESIAN_POINT ( 'NONE',  ( -2.181221257712567141, 23.81760731231018369, 0.2322847663867408652 ) ) ;
#6057 = DIRECTION ( 'NONE',  ( 0.000000000000000000, 1.000000000000000000, 0.000000000000000000 ) ) ;
#6059 = CARTESIAN_POINT ( 'NONE',  ( -2.329590180155310719, 27.99999999999985079, -3.273812635903178059 ) ) ;
#6060 = CARTESIAN_POINT ( 'NONE',  ( 6.164405146010373038, 14.04569583898674523, -0.4648891801310362504 ) ) ;
#6061 = CARTESIAN_POINT ( 'NONE',  ( -23.74465998031000069, -6.216878364870000340, 12.50000000000000000 ) ) ;
#6062 = CARTESIAN_POINT ( 'NONE',  ( 24.48327518124253288, -1.286795374954470939, -12.49999999999999822 ) ) ;
#6063 = VERTEX_POINT ( 'NONE', #2541 ) ;
#6064 = VERTEX_POINT ( 'NONE', #10430 ) ;
#6065 = AXIS2_PLACEMENT_3D ( 'NONE', #5827, #16372, #7165 ) ;
#6066 = CARTESIAN_POINT ( 'NONE',  ( -14.00000000000000355, -9.276317213022405639, -4.032382767787531463 ) ) ;
#6067 = CARTESIAN_POINT ( 'NONE',  ( -9.887017211694999475, -14.92817890949999970, -4.420227885350999308 ) ) ;
#6068 = CARTESIAN_POINT ( 'NONE',  ( -0.6904636124130929531, 6.812739684286071018, -1.608326952461486714 ) ) ;
#6069 = CARTESIAN_POINT ( 'NONE',  ( 0.000000000000000000, 15.00000000000000000, 0.000000000000000000 ) ) ;
#6070 = ORIENTED_EDGE ( 'NONE', *, *, #15908, .T. ) ;
#6071 = CARTESIAN_POINT ( 'NONE',  ( -22.17317987022000025, -9.611087939101999211, -1.202903246196999953 ) ) ;
#6072 = CARTESIAN_POINT ( 'NONE',  ( -14.47125382252185766, 11.86037473473944992, 4.457180938888235744 ) ) ;
#6073 = DIRECTION ( 'NONE',  ( 0.000000000000000000, -1.000000000000000000, 0.000000000000000000 ) ) ;
#6074 = CARTESIAN_POINT ( 'NONE',  ( 15.58068586916286158, -6.908712814867072893, 7.703922221359164269 ) ) ;
#6075 = DIRECTION ( 'NONE',  ( -0.5000000000000169864, 0.000000000000000000, 0.8660254037844289376 ) ) ;
#6076 = EDGE_CURVE ( 'NONE', #19490, #9820, #7375, .T. ) ;
#6077 = CARTESIAN_POINT ( 'NONE',  ( -1.880548603011000131, 29.11986934341000222, -1.127614642727999827 ) ) ;
#6078 = CARTESIAN_POINT ( 'NONE',  ( -19.55887123173999953, -9.833822427806001798, 3.504477313184999776 ) ) ;
#6079 = CARTESIAN_POINT ( 'NONE',  ( -19.53660345378999708, -7.531619525312000185, 7.381236299612999652 ) ) ;
#6080 = CARTESIAN_POINT ( 'NONE',  ( 1.210944093517519971, 29.67954644253612884, 1.788468199683581172 ) ) ;
#6081 = ORIENTED_EDGE ( 'NONE', *, *, #5543, .T. ) ;
#6082 = VECTOR ( 'NONE', #197, 1000.000000000000000 ) ;
#6083 = CARTESIAN_POINT ( 'NONE',  ( -2.013021446580000262, 23.53766161991999795, -0.8520286084860999587 ) ) ;
#6084 = LINE ( 'NONE', #16998, #20483 ) ;
#6085 = ORIENTED_EDGE ( 'NONE', *, *, #5708, .T. ) ;
#6086 = CARTESIAN_POINT ( 'NONE',  ( -3.341782429828001888, 13.63576718287998268, 5.133260327393998068 ) ) ;
#6087 = EDGE_CURVE ( 'NONE', #18500, #18102, #23244, .T. ) ;
#6088 = B_SPLINE_CURVE_WITH_KNOTS ( 'NONE', 3,
 ( #8924, #3475, #23317, #23569, #4931 ),
 .UNSPECIFIED., .F., .F.,
 ( 4, 1, 4 ),
 ( 0.000000000000000000, 0.5000000000000000000, 1.000000000000000000 ),
 .UNSPECIFIED. ) ;
#6089 = CARTESIAN_POINT ( 'NONE',  ( -24.50000000000000000, 3.293267271483000247, -9.759323269498999309 ) ) ;
#6090 = CARTESIAN_POINT ( 'NONE',  ( 18.13612658530999866, 10.25022803218000078, -0.6090841227779000278 ) ) ;
#6091 = ORIENTED_EDGE ( 'NONE', *, *, #23433, .T. ) ;
#6092 = AXIS2_PLACEMENT_3D ( 'NONE', #15113, #3880, #3994 ) ;
#6093 = DIRECTION ( 'NONE',  ( -0.7071067811865474617, -0.7071067811865474617, 0.000000000000000000 ) ) ;
#6094 = DIRECTION ( 'NONE',  ( 1.000000000000000000, 0.000000000000000000, 0.000000000000000000 ) ) ;
#6095 = B_SPLINE_SURFACE_WITH_KNOTS ( 'NONE', 3, 3, ( 
 ( #23859, #14769, #16357, #5690, #22054, #10919, #21932, #5344, #22165, #12618, #12733, #20474, #20127, #5577, #3535, #12955, #11274, #16590, #1600, #20003, #7502, #8985, #5463, #16703, #9212, #12845, #20241, #20354, #3645, #2, #3760, #11149, #1943, #9330, #113 ),
 ( #14884, #3883, #18651, #2058, #16243, #7043, #23635, #7625, #9683, #5920, #6280, #7748, #2407, #11861, #7864, #705, #4238, #11628, #18998, #20584, #15002, #7984, #13665, #15232, #577, #9798, #17184, #8115, #11509, #15114, #16822, #16945, #13549, #347, #11390 ),
 ( #21058, #17305, #15481, #11742, #18885, #20702, #15356, #20825, #9919, #22746, #6163, #20945, #4351, #6037, #19115, #227, #2528, #22399, #17063, #13305, #4471, #22511, #22867, #19243, #22626, #9448, #5810, #13193, #3995, #18760, #2172, #9563, #4111, #13425, #2293 ),
 ( #461, #4723, #8348, #10050, #10169, #6767, #17554, #4600, #17434, #14159, #8230, #21677, #17677, #828, #4845, #1202, #4968, #12354, #15841, #10287, #12231, #11989, #12469, #1326, #12110, #19743, #3153, #1074, #10415, #13784, #21310, #19497, #10536, #17921, #14282 ) ),
 .UNSPECIFIED., .F., .F., .F.,
 ( 4, 4 ),
 ( 4, 1, 1, 1, 1, 1, 1, 1, 1, 1, 1, 1, 1, 1, 1, 1, 1, 1, 1, 1, 1, 1, 1, 1, 1, 1, 1, 1, 1, 1, 1, 1, 4 ),
 ( -0.08408083179840999954, 1.084080831798000188 ),
 ( -0.02000000000000000042, 0.01250000000000000069, 0.04499999999999999833, 0.07749999999999999944, 0.1100000000000000006, 0.1424999999999999878, 0.1749999999999999889, 0.2074999999999999900, 0.2399999999999999911, 0.2725000000000000200, 0.3049999999999999933, 0.3375000000000000222, 0.3699999999999999956, 0.4025000000000000244, 0.4349999999999999978, 0.4675000000000000266, 0.5000000000000000000, 0.5324999999999999734, 0.5649999999999999467, 0.5975000000000000311, 0.6300000000000000044, 0.6624999999999999778, 0.6949999999999999512, 0.7275000000000000355, 0.7600000000000000089, 0.7924999999999999822, 0.8249999999999999556, 0.8575000000000000400, 0.8900000000000000133, 0.9224999999999999867, 0.9549999999999999600, 0.9875000000000000444, 1.020000000000000018 ),
 .UNSPECIFIED. ) ;
#6096 = ORIENTED_EDGE ( 'NONE', *, *, #2904, .F. ) ;
#6097 = DIRECTION ( 'NONE',  ( 0.000000000000000000, -1.000000000000000000, 0.000000000000000000 ) ) ;
#6098 = DIRECTION ( 'NONE',  ( 1.000000000000000000, 0.000000000000000000, 0.000000000000000000 ) ) ;
#6099 = CARTESIAN_POINT ( 'NONE',  ( 4.740896961984002012, 12.61498246287000669, -0.02295444947824999346 ) ) ;
#6100 = CARTESIAN_POINT ( 'NONE',  ( 4.000000000000000000, 26.46241504948189416, 0.8002143650531878816 ) ) ;
#6101 = CARTESIAN_POINT ( 'NONE',  ( 17.89236288313008316, -6.599759852709097707, -8.116454319322453870 ) ) ;
#6102 = AXIS2_PLACEMENT_3D ( 'NONE', #16253, #17848, #14201 ) ;
#6103 = CARTESIAN_POINT ( 'NONE',  ( -23.75392437285000113, 6.466984436016000259, 12.35560119250000000 ) ) ;
#6104 = ADVANCED_FACE ( 'NONE', ( #21570 ), #12369, .T. ) ;
#6105 = CARTESIAN_POINT ( 'NONE',  ( -2.649999999999999911, 26.50000000000000000, 0.000000000000000000 ) ) ;
#6106 = CARTESIAN_POINT ( 'NONE',  ( 2.500000000000000000, 28.63419673618999894, 0.000000000000000000 ) ) ;
#6107 = DIRECTION ( 'NONE',  ( 0.000000000000000000, -0.7746237854577067150, 0.6324223201336057754 ) ) ;
#6108 = CARTESIAN_POINT ( 'NONE',  ( 4.835177208035999818, -12.44999999999999929, 0.000000000000000000 ) ) ;
#6109 = CARTESIAN_POINT ( 'NONE',  ( 14.70899999999999963, -9.048743642952000954, 0.000000000000000000 ) ) ;
#6110 = CARTESIAN_POINT ( 'NONE',  ( -0.06504580400199751200, 30.39993742280512734, 2.159169369958346518 ) ) ;
#6111 = ORIENTED_EDGE ( 'NONE', *, *, #10839, .T. ) ;
#6112 = CARTESIAN_POINT ( 'NONE',  ( -16.59891243917333270, -8.860514229207437253, 2.381066699024747546 ) ) ;
#6113 = CARTESIAN_POINT ( 'NONE',  ( 20.75421567572999848, -2.745092682207000312, -9.410255969462001602 ) ) ;
#6114 = CARTESIAN_POINT ( 'NONE',  ( -0.8045575664689312845, 12.82434487819426572, -6.623413967079410547 ) ) ;
#6115 = CARTESIAN_POINT ( 'NONE',  ( 23.41677564524290744, 37.01856778792605240, 6.000000000000000000 ) ) ;
#6116 = AXIS2_PLACEMENT_3D ( 'NONE', #5936, #2313, #3780 ) ;
#6117 = CARTESIAN_POINT ( 'NONE',  ( -19.89453591501058582, 6.153835458516363488, 8.498639860652758671 ) ) ;
#6118 = CARTESIAN_POINT ( 'NONE',  ( 2.270811333173000435, 26.40614211381999965, -0.3140912549739999782 ) ) ;
#6119 = EDGE_CURVE ( 'NONE', #17324, #12095, #4737, .T. ) ;
#6120 = DIRECTION ( 'NONE',  ( 1.000000000000000000, 0.000000000000000000, 0.000000000000000000 ) ) ;
#6121 = ORIENTED_EDGE ( 'NONE', *, *, #7630, .T. ) ;
#6122 = AXIS2_PLACEMENT_3D ( 'NONE', #1838, #11163, #12747 ) ;
#6123 = CARTESIAN_POINT ( 'NONE',  ( -17.57271597048792700, -9.444424520270592538, 4.430025553576289354 ) ) ;
#6124 = CARTESIAN_POINT ( 'NONE',  ( -3.999702431747993003, 24.50639765414745241, -0.3779811684369214220 ) ) ;
#6125 = AXIS2_PLACEMENT_3D ( 'NONE', #9671, #7736, #22497 ) ;
#6126 = CIRCLE ( 'NONE', #4590, 4.000000000000000000 ) ;
#6127 = CARTESIAN_POINT ( 'NONE',  ( -1.047143917943662350, 27.76680419753780527, 1.933088563971394613 ) ) ;
#6128 = CARTESIAN_POINT ( 'NONE',  ( -12.25000000000000000, 1.374666032043000015E-14, 0.000000000000000000 ) ) ;
#6129 = ORIENTED_EDGE ( 'NONE', *, *, #14833, .T. ) ;
#6130 = CARTESIAN_POINT ( 'NONE',  ( 16.99624770046333921, -7.283006694536083181, -5.596856954334615608 ) ) ;
#6131 = VECTOR ( 'NONE', #19108, 1000.000000000000227 ) ;
#6132 = CARTESIAN_POINT ( 'NONE',  ( 17.17537674931000069, -4.906342569036000079, 9.567493125660998743 ) ) ;
#6133 = EDGE_CURVE ( 'NONE', #19752, #9155, #10038, .T. ) ;
#6134 = CARTESIAN_POINT ( 'NONE',  ( -19.21948930940000011, -9.233400656586999489, -6.760258690304999263 ) ) ;
#6135 = DIRECTION ( 'NONE',  ( -0.000000000000000000, 1.000000000000000000, 0.000000000000000000 ) ) ;
#6136 = EDGE_CURVE ( 'NONE', #16360, #11502, #1539, .T. ) ;
#6137 = CARTESIAN_POINT ( 'NONE',  ( 15.86921080085999769, -10.66112877511999990, -3.930111991920000047 ) ) ;
#6138 = CARTESIAN_POINT ( 'NONE',  ( 13.50000000000000000, -8.269916559704732606, -4.425252021080920528 ) ) ;
#6139 = CARTESIAN_POINT ( 'NONE',  ( 0.000000000000000000, 20.10000000000000142, 0.000000000000000000 ) ) ;
#6140 = CARTESIAN_POINT ( 'NONE',  ( 25.09343792058000133, -5.309646865108000213, 8.124620694544001154 ) ) ;
#6141 = VECTOR ( 'NONE', #13930, 1000.000000000000000 ) ;
#6142 = CARTESIAN_POINT ( 'NONE',  ( 3.999895459877826465, 24.70780860099995380, -1.909390889640790512 ) ) ;
#6143 = VERTEX_POINT ( 'NONE', #23362 ) ;
#6144 = CARTESIAN_POINT ( 'NONE',  ( 12.61436189658999929, 4.419636859381000704, -7.963858022973001383 ) ) ;
#6145 = CARTESIAN_POINT ( 'NONE',  ( -2.030073792688000367, 27.06456776951999998, -1.733846816783999989 ) ) ;
#6146 = TOROIDAL_SURFACE ( 'NONE', #20853, 3.000000000000000000, 1.000000000000000000 ) ;
#6147 = CARTESIAN_POINT ( 'NONE',  ( 4.392057029119999179, 12.33170126310999670, 1.899976486714999746 ) ) ;
#6148 = CARTESIAN_POINT ( 'NONE',  ( 2.095699401784793192, 28.97244882208192607, 0.5250962896352469045 ) ) ;
#6149 = CARTESIAN_POINT ( 'NONE',  ( -19.78402572227999912, 1.667133957923000009, 10.91833191109000012 ) ) ;
#6150 = ORIENTED_EDGE ( 'NONE', *, *, #7770, .T. ) ;
#6151 = ADVANCED_FACE ( 'NONE', ( #23617, #2919 ), #17820, .T. ) ;
#6152 = EDGE_CURVE ( 'NONE', #12183, #20328, #16031, .T. ) ;
#6153 = DIRECTION ( 'NONE',  ( 1.000000000000000000, 0.000000000000000000, 0.000000000000000000 ) ) ;
#6154 = AXIS2_PLACEMENT_3D ( 'NONE', #3836, #17142, #19072 ) ;
#6155 = ORIENTED_EDGE ( 'NONE', *, *, #14821, .F. ) ;
#6156 = CARTESIAN_POINT ( 'NONE',  ( -24.50000000000000000, 0.000000000000000000, -12.50000000000000000 ) ) ;
#6157 = CARTESIAN_POINT ( 'NONE',  ( -2.921311158041803413, 11.94552971169360589, 3.795700454126800238 ) ) ;
#6158 = CARTESIAN_POINT ( 'NONE',  ( 1.332518472557000067, 27.97049822781000117, 1.834054417453000019 ) ) ;
#6159 = CARTESIAN_POINT ( 'NONE',  ( 4.918565628415999313, 13.52958698473998567, 5.101225743681996327 ) ) ;
#6160 = CARTESIAN_POINT ( 'NONE',  ( 0.5400519283707410079, 6.798561526091877916, 1.667608383989048759 ) ) ;
#6161 = CARTESIAN_POINT ( 'NONE',  ( 13.55568924931000119, -5.133899498893999436, 9.338903284905999413 ) ) ;
#6162 = VECTOR ( 'NONE', #20377, 1000.000000000000000 ) ;
#6163 = CARTESIAN_POINT ( 'NONE',  ( -17.46454189286000158, -8.119858849493999386, 7.209780893148999503 ) ) ;
#6164 = CIRCLE ( 'NONE', #19731, 2.000000000000000000 ) ;
#6165 = CARTESIAN_POINT ( 'NONE',  ( 12.16012625731000085, 8.900490462747001175, -1.861105101465000189 ) ) ;
#6166 = VECTOR ( 'NONE', #1123, 1000.000000000000000 ) ;
#6167 = CARTESIAN_POINT ( 'NONE',  ( 24.45564077607145492, 11.85537957198067005, -4.465880238315118156 ) ) ;
#6168 = ORIENTED_EDGE ( 'NONE', *, *, #50, .F. ) ;
#6169 = CARTESIAN_POINT ( 'NONE',  ( -2.704380769729999745, 30.47523026870999985, 0.3249933680386999924 ) ) ;
#6170 = B_SPLINE_CURVE_WITH_KNOTS ( 'NONE', 3,
 ( #16410, #5631, #1888, #7209, #13014, #3823, #16534, #2005, #23921, #9389, #16761, #21995, #11338, #12793, #170, #5410, #7561, #13255 ),
 .UNSPECIFIED., .F., .F.,
 ( 4, 2, 2, 2, 2, 2, 2, 2, 4 ),
 ( 0.000000000000000000, 0.1250000000000000000, 0.2500000000000000000, 0.3750000000000000000, 0.5000000000000000000, 0.6250000000000000000, 0.7500000000000000000, 0.8750000000000000000, 1.000000000000000000 ),
 .UNSPECIFIED. ) ;
#6171 = CARTESIAN_POINT ( 'NONE',  ( -2.573651909687999950, 24.13278196464000303, -0.8679085051213999424 ) ) ;
#6172 = CARTESIAN_POINT ( 'NONE',  ( 14.02876822787055033, -10.30979721075241073, -0.6943530198432756873 ) ) ;
#6173 = ORIENTED_EDGE ( 'NONE', *, *, #19301, .F. ) ;
#6174 = CARTESIAN_POINT ( 'NONE',  ( -2.256930243168998818, 12.92976665894000732, -6.094107447253994891 ) ) ;
#6175 = CARTESIAN_POINT ( 'NONE',  ( 30.87226923053214378, 35.51856778792605240, -2.673746900119611247 ) ) ;
#6176 = CARTESIAN_POINT ( 'NONE',  ( -2.296046026427999820, 29.04809310863999627, 1.505608598421000144 ) ) ;
#6177 = CARTESIAN_POINT ( 'NONE',  ( 11.48478210364236674, 3.271710350470132589, 12.49991250862224490 ) ) ;
#6178 = CARTESIAN_POINT ( 'NONE',  ( 18.79674436531792736, 0.1206336078962078756, 10.48047579883863989 ) ) ;
#6179 = DIRECTION ( 'NONE',  ( 0.000000000000000000, -1.000000000000000000, 0.000000000000000000 ) ) ;
#6180 = CARTESIAN_POINT ( 'NONE',  ( -21.24728743917332352, 7.370242396797828555, -5.663897891694076314 ) ) ;
#6181 = CARTESIAN_POINT ( 'NONE',  ( 23.99999963380687618, 13.93375672974000246, -1.355252715606880543E-17 ) ) ;
#6182 = ORIENTED_EDGE ( 'NONE', *, *, #23738, .T. ) ;
#6183 = CARTESIAN_POINT ( 'NONE',  ( 11.72559253312535432, -8.766982473567979994, 9.815058145095289177 ) ) ;
#6184 = EDGE_LOOP ( 'NONE', ( #15415, #17829, #15750, #610, #5579, #20497, #14952, #1323 ) ) ;
#6185 = LINE ( 'NONE', #12013, #23825 ) ;
#6187 = CARTESIAN_POINT ( 'NONE',  ( 2.500000000000001776, 28.61753006952332967, 0.3272492347489252551 ) ) ;
#6186 = CARTESIAN_POINT ( 'NONE',  ( -4.772412363876479269, 12.42044774334072166, 0.8590728381116085055 ) ) ;
#6188 = CARTESIAN_POINT ( 'NONE',  ( -23.76320767108999732, -6.966447585166999801, -12.06723600888999925 ) ) ;
#6189 = CARTESIAN_POINT ( 'NONE',  ( 15.31342757799999887, 6.394788428435000505, 8.996804509239000325 ) ) ;
#6190 = CARTESIAN_POINT ( 'NONE',  ( -7.088468813309002137, 15.38200575439001128, -1.346721112802998332 ) ) ;
#6191 = PRODUCT_DEFINITION ( 'UNKNOWN', '', #17144, #16438 ) ;
#6192 = LINE ( 'NONE', #13577, #13642 ) ;
#6193 = VERTEX_POINT ( 'NONE', #10180 ) ;
#6194 = ORIENTED_EDGE ( 'NONE', *, *, #15472, .T. ) ;
#6195 = CARTESIAN_POINT ( 'NONE',  ( -24.17970357207700260, 8.771272208504171886, -9.807700027458217562 ) ) ;
#6196 = CARTESIAN_POINT ( 'NONE',  ( -0.9206838382964129819, 6.836823221689457775, -1.505541136744114938 ) ) ;
#6197 = CARTESIAN_POINT ( 'NONE',  ( -14.45960647534970178, -9.597314625688284195, -8.376896358978855872 ) ) ;
#6198 = VERTEX_POINT ( 'NONE', #6780 ) ;
#6199 = CARTESIAN_POINT ( 'NONE',  ( 1.764297223473136000, 13.00000000000000000, -1.071763214071401515 ) ) ;
#6200 = CARTESIAN_POINT ( 'NONE',  ( 6.220388596125608238, 13.78688666331658830, 1.207122575335724424 ) ) ;
#6201 = CARTESIAN_POINT ( 'NONE',  ( 15.25236472003948940, 4.074645878791661069, 9.504836835712692888 ) ) ;
#6202 = CARTESIAN_POINT ( 'NONE',  ( -19.60935064726000121, -11.08680168281000000, 1.130667934175000111 ) ) ;
#6203 = CARTESIAN_POINT ( 'NONE',  ( -9.000000000000000000, 18.50000000000000000, -5.000000000000000000 ) ) ;
#6204 = CARTESIAN_POINT ( 'NONE',  ( -20.84460765454501185, -0.9149537475125872898, -10.47345582031393896 ) ) ;
#6205 = CARTESIAN_POINT ( 'NONE',  ( -15.43323841317000067, -10.79835415318000003, -0.2870680789784999520 ) ) ;
#6206 = CARTESIAN_POINT ( 'NONE',  ( -1.099135848509952051, 29.53578701925532357, 1.859266377551254346 ) ) ;
#6207 = ORIENTED_EDGE ( 'NONE', *, *, #5798, .F. ) ;
#6208 = CARTESIAN_POINT ( 'NONE',  ( 1.453244340366000031, 24.09604374391000192, -1.632848260547999919 ) ) ;
#6209 = DIRECTION ( 'NONE',  ( -1.000000000000000000, 0.000000000000000000, 0.000000000000000000 ) ) ;
#6210 = CIRCLE ( 'NONE', #19775, 2.949999999999999734 ) ;
#6211 = ORIENTED_EDGE ( 'NONE', *, *, #22377, .F. ) ;
#6212 = CARTESIAN_POINT ( 'NONE',  ( -23.74465998031000069, 7.716878364870000340, -11.63397459621999985 ) ) ;
#6213 = CARTESIAN_POINT ( 'NONE',  ( 5.899122318018997113, 14.55469254769999488, -1.683791433005999760 ) ) ;
#6214 = DIRECTION ( 'NONE',  ( 0.000000000000000000, 0.000000000000000000, 1.000000000000000000 ) ) ;
#6215 = B_SPLINE_CURVE_WITH_KNOTS ( 'NONE', 3,
 ( #19772, #15870, #3060, #18197, #3182 ),
 .UNSPECIFIED., .F., .F.,
 ( 4, 1, 4 ),
 ( 0.000000000000000000, 0.5000000000000000000, 1.000000000000000000 ),
 .UNSPECIFIED. ) ;
#6216 = CARTESIAN_POINT ( 'NONE',  ( -24.50000000000000000, -1.873582633960999999, -10.39897383761999983 ) ) ;
#6217 = ADVANCED_FACE ( 'NONE', ( #19757 ), #4982, .T. ) ;
#6218 = CARTESIAN_POINT ( 'NONE',  ( 18.24581408530999838, 9.747919580236001025, 3.236577786812999680 ) ) ;
#6219 = VERTEX_POINT ( 'NONE', #1091 ) ;
#6220 = CARTESIAN_POINT ( 'NONE',  ( -6.250000000000000000, 1.301187224093999891E-14, 0.000000000000000000 ) ) ;
#6221 = CARTESIAN_POINT ( 'NONE',  ( 0.000000000000000000, 0.000000000000000000, 0.000000000000000000 ) ) ;
#6222 = CYLINDRICAL_SURFACE ( 'NONE', #19982, 15.43375672974000068 ) ;
#6223 = ORIENTED_EDGE ( 'NONE', *, *, #81, .F. ) ;
#6224 = CARTESIAN_POINT ( 'NONE',  ( -12.50000000000000000, 6.965460728298000781, -5.686777139159000072 ) ) ;
#6225 = DIRECTION ( 'NONE',  ( -1.000000000000000000, 0.000000000000000000, 0.000000000000000000 ) ) ;
#6226 = CARTESIAN_POINT ( 'NONE',  ( -23.39099967059616958, 6.713552081593185505, -6.458098826819107963 ) ) ;
#6227 = CARTESIAN_POINT ( 'NONE',  ( -12.50000000000000000, 1.377727649040999975E-14, 0.000000000000000000 ) ) ;
#6228 = CARTESIAN_POINT ( 'NONE',  ( 18.40433895126197683, 9.206357412411914964, -4.883359051719883936 ) ) ;
#6229 = CARTESIAN_POINT ( 'NONE',  ( 0.000000000000000000, 17.00000000000000000, 0.000000000000000000 ) ) ;
#6230 = ADVANCED_FACE ( 'NONE', ( #1340 ), #23182, .F. ) ;
#6231 = CARTESIAN_POINT ( 'NONE',  ( -14.40719418339326729, 8.953944931993316203, -9.491079701373065447 ) ) ;
#6232 = CARTESIAN_POINT ( 'NONE',  ( -5.090709799003004576, 16.33848066163001889, -3.590694264005000136 ) ) ;
#6233 = DIRECTION ( 'NONE',  ( -0.7071067811865975328, -0.7071067811864976127, -1.204881101557994910E-09 ) ) ;
#6234 = CARTESIAN_POINT ( 'NONE',  ( -2.500000000000000888, 29.01753006952332825, -0.3272492347489316944 ) ) ;
#6235 = DIRECTION ( 'NONE',  ( 0.000000000000000000, 1.000000000000000000, 0.000000000000000000 ) ) ;
#6236 = CARTESIAN_POINT ( 'NONE',  ( 2.140330047059040730, 30.58679688062958846, 0.2894183440755233039 ) ) ;
#6237 = EDGE_LOOP ( 'NONE', ( #15655, #9289, #9947, #16870 ) ) ;
#6238 = CARTESIAN_POINT ( 'NONE',  ( 19.31333166812999735, -6.932005976255000590, -8.325654194909999362 ) ) ;
#6239 = CARTESIAN_POINT ( 'NONE',  ( -4.227279577313947101, 13.39853892358859433, -5.369578654743469848 ) ) ;
#6240 = CARTESIAN_POINT ( 'NONE',  ( 1.055729715565287385, 29.92936170367563520, 4.009276318043865750 ) ) ;
#6241 = CARTESIAN_POINT ( 'NONE',  ( -19.97486504007325436, 8.250260110346381737, 6.482288355094454779 ) ) ;
#6242 = CARTESIAN_POINT ( 'NONE',  ( 1.120191590154000050, 25.72364211381999866, -2.000256872718999990 ) ) ;
#6243 = CARTESIAN_POINT ( 'NONE',  ( 0.000000000000000000, 18.00000000000000000, 0.000000000000000000 ) ) ;
#6244 = VERTEX_POINT ( 'NONE', #21690 ) ;
#6245 = EDGE_CURVE ( 'NONE', #1842, #8248, #5909, .T. ) ;
#6246 = CARTESIAN_POINT ( 'NONE',  ( -17.07031370036265017, -2.772578259958148550, -10.04572367896972906 ) ) ;
#6247 = CARTESIAN_POINT ( 'NONE',  ( -4.000000000000115463, 24.49999999999976197, -0.1904558375376560198 ) ) ;
#6248 = CARTESIAN_POINT ( 'NONE',  ( -2.199358294017834670, 28.43250573243029322, 0.04245723217612143441 ) ) ;
#6249 = EDGE_LOOP ( 'NONE', ( #598, #23358, #516, #22683 ) ) ;
#6250 = VERTEX_POINT ( 'NONE', #16801 ) ;
#6251 = DIRECTION ( 'NONE',  ( 0.000000000000000000, -1.000000000000000000, 0.000000000000000000 ) ) ;
#6252 = CARTESIAN_POINT ( 'NONE',  ( 11.88393908531000065, -9.721606288483000569, -2.753149205743999683 ) ) ;
#6253 = CARTESIAN_POINT ( 'NONE',  ( -22.77424452324999748, -7.081648116287999173, -8.665291262669999384 ) ) ;
#6254 = EDGE_CURVE ( 'NONE', #2037, #9910, #7601, .T. ) ;
#6255 = CARTESIAN_POINT ( 'NONE',  ( -13.12557887030999915, 10.05389705766999953, -2.585396581761999713 ) ) ;
#6256 = FACE_BOUND ( 'NONE', #19308, .T. ) ;
#6257 = CARTESIAN_POINT ( 'NONE',  ( 14.04108580085999947, -10.79197239458999924, -3.388753120225000082 ) ) ;
#6258 = CARTESIAN_POINT ( 'NONE',  ( -1.928881730073939371, 28.53949304903204265, -1.071374732005587527 ) ) ;
#6259 = DIRECTION ( 'NONE',  ( 0.9989428060277519839, 0.000000000000000000, -0.04597031961386779941 ) ) ;
#6260 = CARTESIAN_POINT ( 'NONE',  ( 25.36474249277999959, -5.041558719633999708, 7.714402359875999871 ) ) ;
#6261 = B_SPLINE_CURVE_WITH_KNOTS ( 'NONE', 3,
 ( #13082, #4246, #19004, #3890, #586, #10058, #836, #21562, #10176, #14167, #10543, #13672, #15963, #8601, #4977, #2665, #19381, #11869, #17928, #1335, #2792, #21317, #23357, #13793, #8722, #10423, #8238, #17441, #12118, #21066, #19253, #10296, #23237, #17563, #21194, #4480, #15606, #11996, #4608, #4732, #22991, #958, #19504, #6774, #16086, #17685, #8356, #12362, #15722, #6410, #19750, #17814, #1084, #6651, #2913, #23113, #6537, #3161 ),
 .UNSPECIFIED., .F., .F.,
 ( 4, 2, 2, 2, 1, 1, 2, 2, 2, 2, 1, 1, 1, 2, 2, 2, 2, 1, 1, 2, 2, 2, 1, 1, 2, 2, 2, 2, 2, 1, 1, 1, 2, 2, 4 ),
 ( 0.000000000000000000, 0.06249999999999863998, 0.09374999999999787670, 0.1093749999999975575, 0.1171874999999975020, 0.1210937499999974604, 0.1230468749999975020, 0.1249999999999975298, 0.1874999999999997502, 0.2187500000000008882, 0.2343750000000013323, 0.2421875000000015543, 0.2460937500000017486, 0.2480468750000016931, 0.2500000000000016098, 0.3125000000000025535, 0.3437500000000031086, 0.3593750000000033862, 0.3671875000000035527, 0.3710937500000035527, 0.3750000000000034972, 0.4375000000000021649, 0.4687500000000014988, 0.4843750000000012212, 0.4921875000000011102, 0.5000000000000009992, 0.7499999999999970024, 0.8124999999999960032, 0.8437499999999955591, 0.8593749999999952260, 0.8671874999999951150, 0.8710937499999951150, 0.8730468749999953371, 0.8749999999999954481, 1.000000000000000000 ),
 .UNSPECIFIED. ) ;
#6262 = CARTESIAN_POINT ( 'NONE',  ( -1.618278083580495963, 26.52244509682108742, -1.955444531118598173 ) ) ;
#6263 = VERTEX_POINT ( 'NONE', #14864 ) ;
#6264 = CARTESIAN_POINT ( 'NONE',  ( -12.00000000000000000, 1.554281285376986145E-14, -7.000000000000000000 ) ) ;
#6265 = CARTESIAN_POINT ( 'NONE',  ( 1.569224139466999901, 28.23456776952000169, 2.159851832628000068 ) ) ;
#6266 = CIRCLE ( 'NONE', #23295, 3.000000000000000000 ) ;
#6267 = CARTESIAN_POINT ( 'NONE',  ( -1.925363223002000357, 11.65848132151000094, 4.402296118137997816 ) ) ;
#6268 = EDGE_CURVE ( 'NONE', #6055, #6143, #18181, .T. ) ;
#6269 = CARTESIAN_POINT ( 'NONE',  ( 2.063594504837999888E-14, 28.80370090847999975, 2.160000000000000142 ) ) ;
#6270 = CARTESIAN_POINT ( 'NONE',  ( -21.26732368540999829, -11.05878950324999899, 0.7642943787211000650 ) ) ;
#6271 = ORIENTED_EDGE ( 'NONE', *, *, #22945, .F. ) ;
#6272 = CARTESIAN_POINT ( 'NONE',  ( -6.180252273306864552, 27.99999999999999645, 1.080215919051256579 ) ) ;
#6273 = VERTEX_POINT ( 'NONE', #11129 ) ;
#6274 = ADVANCED_FACE ( 'NONE', ( #5217 ), #8507, .T. ) ;
#6275 = DIRECTION ( 'NONE',  ( 0.000000000000000000, 0.000000000000000000, -1.000000000000000000 ) ) ;
#6276 = CARTESIAN_POINT ( 'NONE',  ( 5.267359632244998480, 13.90542513608999897, 3.709429151287999105 ) ) ;
#6277 = EDGE_CURVE ( 'NONE', #17401, #23059, #12829, .T. ) ;
#6278 = CARTESIAN_POINT ( 'NONE',  ( -1.750000000000000222, 7.000000000000004441, 0.1353757534095987036 ) ) ;
#6279 = DIRECTION ( 'NONE',  ( -1.000000000000000000, 0.000000000000000000, 0.000000000000000000 ) ) ;
#6280 = CARTESIAN_POINT ( 'NONE',  ( -17.22065346366999705, -7.714380452752999773, 6.849660182178999968 ) ) ;
#6281 = AXIS2_PLACEMENT_3D ( 'NONE', #1112, #17216, #19150 ) ;
#6282 = CARTESIAN_POINT ( 'NONE',  ( 12.26981375731000057, 8.958847990383999260, 1.572873132563999965 ) ) ;
#6283 = CARTESIAN_POINT ( 'NONE',  ( 24.37713355803437665, 2.989142673506741232, 12.50000000000000355 ) ) ;
#6284 = ORIENTED_EDGE ( 'NONE', *, *, #20319, .F. ) ;
#6285 = EDGE_CURVE ( 'NONE', #17341, #23303, #15829, .T. ) ;
#6286 = CARTESIAN_POINT ( 'NONE',  ( 20.32323479018660706, 8.891074209933115924, 5.624032425053880679 ) ) ;
#6287 = CARTESIAN_POINT ( 'NONE',  ( 12.52688711657000020, -13.93375672974000068, -0.8660254037843999608 ) ) ;
#6288 = EDGE_CURVE ( 'NONE', #2693, #13406, #14637, .T. ) ;
#6289 = CARTESIAN_POINT ( 'NONE',  ( -0.3515821444375999971, 23.66184656560000121, 2.500975805065000390 ) ) ;
#6290 = CARTESIAN_POINT ( 'NONE',  ( 0.000000000000000000, 15.00000000000000000, -2.704938617610999654E-14 ) ) ;
#6291 = ORIENTED_EDGE ( 'NONE', *, *, #11500, .F. ) ;
#6292 = CARTESIAN_POINT ( 'NONE',  ( -3.963089716433997101, 14.56865066125998709, -4.679596269295001498 ) ) ;
#6293 =( LENGTH_UNIT ( ) NAMED_UNIT ( * ) SI_UNIT ( .MILLI., .METRE. ) );
#6294 = DIRECTION ( 'NONE',  ( 0.000000000000000000, 1.000000000000000000, 0.000000000000000000 ) ) ;
#6295 = CARTESIAN_POINT ( 'NONE',  ( 12.52688711657000020, -6.216878364870000340, 12.50000000000000000 ) ) ;
#6296 = CARTESIAN_POINT ( 'NONE',  ( 18.46221799045618184, 9.641442781986372168, 4.082290055557257880 ) ) ;
#6297 = DIRECTION ( 'NONE',  ( -1.000000000000000000, 0.000000000000000000, 0.000000000000000000 ) ) ;
#6298 = CARTESIAN_POINT ( 'NONE',  ( 0.3272492347489341924, 29.61753006952334033, -2.500000000000000888 ) ) ;
#6299 = ORIENTED_EDGE ( 'NONE', *, *, #7750, .F. ) ;
#6300 = DIRECTION ( 'NONE',  ( 0.000000000000000000, 0.7071067811866525998, -0.7071067811864425456 ) ) ;
#6301 = CARTESIAN_POINT ( 'NONE',  ( 4.623021688823209630, 12.49842695769186740, -1.256073083333553830 ) ) ;
#6302 = ORIENTED_EDGE ( 'NONE', *, *, #7433, .T. ) ;
#6303 = B_SPLINE_SURFACE_WITH_KNOTS ( 'NONE', 3, 3, ( 
 ( #13153, #5881, #11233, #11700, #539, #11584, #2016, #20545, #22229, #5994, #15193, #18611, #7944, #18959, #16774, #15309, #13379, #422, #4309, #6113, #2488, #4187, #9877, #11348, #20781, #4071, #17263, #7454, #14837, #2367, #18841, #11463, #183, #7573, #14953 ),
 ( #22349, #18720, #2130, #9519, #16896, #299, #15075, #13266, #20660, #2245, #9639, #17023, #8306, #10369, #15555, #8432, #21018, #2979, #1162, #2860, #13870, #22942, #15671, #12306, #23060, #23305, #4430, #21140, #8556, #11820, #2742, #10122, #21273, #2612, #13620 ),
 ( #4682, #6488, #10243, #10001, #4800, #10496, #12069, #1030, #17759, #19452, #15799, #19198, #19331, #17511, #15914, #6722, #19696, #905, #23191, #17392, #11946, #4920, #22824, #14113, #4555, #787, #19574, #17633, #6359, #6238, #6608, #8187, #21508, #13991, #13741 ),
 ( #21385, #3112, #662, #8068, #15437, #12185, #18666, #21749, #14236, #18120, #12432, #9463, #20492, #16839, #8915, #1958, #2073, #10612, #5590, #14782, #3778, #12544, #16156, #8794, #16717, #243, #10728, #1282, #1526, #9344, #5162, #128, #13208, #18553, #5050 ) ),
 .UNSPECIFIED., .F., .F., .F.,
 ( 4, 4 ),
 ( 4, 1, 1, 1, 1, 1, 1, 1, 1, 1, 1, 1, 1, 1, 1, 1, 1, 1, 1, 1, 1, 1, 1, 1, 1, 1, 1, 1, 1, 1, 1, 1, 4 ),
 ( -0.08331297109794999489, 1.083312971098000066 ),
 ( 0.1014657448152999908, 0.1300955127501000064, 0.1587252806848999942, 0.1873550486197999854, 0.2159848165546000009, 0.2446145844893999888, 0.2732443524242000321, 0.3018741203590000199, 0.3305038882938000078, 0.3591336562285999956, 0.3877634241634000389, 0.4163931920982000268, 0.4450229600330000146, 0.4736527279678000024, 0.5022824959025999902, 0.5309122638374000891, 0.5595420317721999659, 0.5881717997070000647, 0.6168015676417999416, 0.6454313355766000404, 0.6740611035114000282, 0.7026908714463000472, 0.7313206393811000350, 0.7599504073159000228, 0.7885801752507000106, 0.8172099431854999985, 0.8458397111202999863, 0.8744694790551000851, 0.9030992469899000730, 0.9317290149246999498, 0.9603587828595000486, 0.9889885507942999254, 1.017618318728999993 ),
 .UNSPECIFIED. ) ;
#6304 = CARTESIAN_POINT ( 'NONE',  ( -5.769429997167383029, 16.25870916169602509, -2.056550855362532015 ) ) ;
#6306 = LINE ( 'NONE', #2809, #12077 ) ;
#6305 = CARTESIAN_POINT ( 'NONE',  ( 0.5498409912916205622, 11.49495375948718490, 4.782145214771198027 ) ) ;
#6307 = CARTESIAN_POINT ( 'NONE',  ( -2.056952183161803394, 12.94126637194106877, 6.392751251890534725 ) ) ;
#6308 = DIRECTION ( 'NONE',  ( 0.000000000000000000, 0.000000000000000000, 1.000000000000000000 ) ) ;
#6309 = CARTESIAN_POINT ( 'NONE',  ( -20.62057330634167940, 0.5096360985298603596, 9.248796765395695729 ) ) ;
#6310 = CARTESIAN_POINT ( 'NONE',  ( 1.402946323589000066, 25.50919433610000198, -2.505154520421000175 ) ) ;
#6311 = ORIENTED_EDGE ( 'NONE', *, *, #3356, .T. ) ;
#6312 = ORIENTED_EDGE ( 'NONE', *, *, #20620, .T. ) ;
#6313 = CARTESIAN_POINT ( 'NONE',  ( -13.99999999999999822, -7.572152359989809511, -6.464702211010298072 ) ) ;
#6314 = CARTESIAN_POINT ( 'NONE',  ( 4.000000000000000000, 24.80000000000000426, 2.309401076759000304 ) ) ;
#6315 = FACE_OUTER_BOUND ( 'NONE', #6551, .T. ) ;
#6316 = EDGE_LOOP ( 'NONE', ( #17035, #1899, #16159, #16856, #9023 ) ) ;
#6317 = EDGE_CURVE ( 'NONE', #2821, #19900, #14874, .T. ) ;
#6318 = CARTESIAN_POINT ( 'NONE',  ( -23.95936891989000017, -4.964537398340999275, -8.976378852492999272 ) ) ;
#6319 = CARTESIAN_POINT ( 'NONE',  ( 1.727213515435479740, 12.96860573960580254, -1.061287104562887551 ) ) ;
#6320 = CARTESIAN_POINT ( 'NONE',  ( 6.190667799111778891, 13.91886042571875670, 0.7936539895852133819 ) ) ;
#6321 = CARTESIAN_POINT ( 'NONE',  ( 15.61445477932001502, -7.782978770127811252, 6.824697942149217766 ) ) ;
#6322 = CARTESIAN_POINT ( 'NONE',  ( -17.11410595495999942, 1.976719737850999969, -10.89867228117000053 ) ) ;
#6323 = DIRECTION ( 'NONE',  ( -0.9999999999999998890, 9.268912834351999024E-09, -3.975900789814998879E-09 ) ) ;
#6324 = CARTESIAN_POINT ( 'NONE',  ( -21.30783991800640464, -10.44792467106556977, 1.268519232389238693 ) ) ;
#6325 = B_SPLINE_CURVE_WITH_KNOTS ( 'NONE', 3,
 ( #17127, #8046, #523, #7926, #15293, #4294 ),
 .UNSPECIFIED., .F., .F.,
 ( 4, 1, 1, 4 ),
 ( 0.000000000000000000, 0.3333333333333000081, 0.6666666666667000474, 1.000000000000000000 ),
 .UNSPECIFIED. ) ;
#6326 = VECTOR ( 'NONE', #10861, 1000.000000000000000 ) ;
#6327 = CARTESIAN_POINT ( 'NONE',  ( -24.05763402810364937, -5.201095832796127638, -8.431872254508961717 ) ) ;
#6328 = CIRCLE ( 'NONE', #17557, 1.000000000000000888 ) ;
#6329 = CARTESIAN_POINT ( 'NONE',  ( -1.856047877541181279, 29.47208282624109543, 1.104794950165609801 ) ) ;
#6330 = VERTEX_POINT ( 'NONE', #10901 ) ;
#6331 = CARTESIAN_POINT ( 'NONE',  ( -1.735522259956000068, 24.30543704041000197, -1.328937561357000030 ) ) ;
#6332 = CARTESIAN_POINT ( 'NONE',  ( -16.48875683979265361, 6.849824468384817067, 8.049161493870508721 ) ) ;
#6333 = ORIENTED_EDGE ( 'NONE', *, *, #21116, .F. ) ;
#6334 = CARTESIAN_POINT ( 'NONE',  ( -4.724999978625000097, 14.90000002138000035, -2.519184009061999785E-09 ) ) ;
#6335 = CARTESIAN_POINT ( 'NONE',  ( 6.081505281638999172, 14.07690835503000493, 0.05978829213082002131 ) ) ;
#6336 = CARTESIAN_POINT ( 'NONE',  ( 12.00000000000000178, -1.529947326563451560, -8.848046545010550545 ) ) ;
#6337 = CYLINDRICAL_SURFACE ( 'NONE', #4124, 2.750000000000000000 ) ;
#6338 = VECTOR ( 'NONE', #6233, 1000.000000000000114 ) ;
#6339 = CARTESIAN_POINT ( 'NONE',  ( 17.25862658530999738, -10.23584709072999921, -0.4386478486912999686 ) ) ;
#6340 = ORIENTED_EDGE ( 'NONE', *, *, #6133, .F. ) ;
#6341 = CARTESIAN_POINT ( 'NONE',  ( -6.297602208228999743, 15.63806030118000656, -1.260321238843998604 ) ) ;
#6342 = CARTESIAN_POINT ( 'NONE',  ( 23.41677564524290744, 34.01856778792605240, 6.000000000000005329 ) ) ;
#6343 = CARTESIAN_POINT ( 'NONE',  ( 0.000000000000000000, 15.00000000000000000, 0.000000000000000000 ) ) ;
#6344 = ORIENTED_EDGE ( 'NONE', *, *, #18262, .F. ) ;
#6345 = DIRECTION ( 'NONE',  ( 0.000000000000000000, -1.000000000000000000, 6.254561278617999028E-11 ) ) ;
#6346 = CARTESIAN_POINT ( 'NONE',  ( 11.70388046502542245, 8.799739770623126844, 9.758286884852591214 ) ) ;
#6347 = VECTOR ( 'NONE', #4693, 1000.000000000000000 ) ;
#6348 = CARTESIAN_POINT ( 'NONE',  ( 22.35132670216752260, 35.07441746931966975, 6.000000000000000000 ) ) ;
#6349 = CARTESIAN_POINT ( 'NONE',  ( -7.034000000000000696, -11.50000000000000000, -2.869685045148000171E-11 ) ) ;
#6350 = CARTESIAN_POINT ( 'NONE',  ( 18.40159154013413811, 9.157578505391652968, -4.974487616550520741 ) ) ;
#6351 = DIRECTION ( 'NONE',  ( 0.000000000000000000, 1.000000000000000000, 0.000000000000000000 ) ) ;
#6352 = CARTESIAN_POINT ( 'NONE',  ( -14.25243324638999809, 13.93375672974000068, -0.8660254037843999608 ) ) ;
#6353 = CARTESIAN_POINT ( 'NONE',  ( 23.39170489349999826, 6.484734603292000799, -9.235218885525998900 ) ) ;
#6354 = CARTESIAN_POINT ( 'NONE',  ( 0.000000000000000000, 20.00000000000000000, 0.000000000000000000 ) ) ;
#6355 = CARTESIAN_POINT ( 'NONE',  ( -4.029105800529611869, 13.82458363547321589, -4.859102542853258377 ) ) ;
#6356 = ADVANCED_FACE ( 'NONE', ( #14751 ), #8966, .T. ) ;
#6357 = CARTESIAN_POINT ( 'NONE',  ( -2.061598702545497375, 30.16504885856303630, -0.6499987980253106867 ) ) ;
#6358 = ORIENTED_EDGE ( 'NONE', *, *, #9766, .F. ) ;
#6359 = CARTESIAN_POINT ( 'NONE',  ( 19.50658260167999813, -0.2703046275102000129, -10.83567124763000145 ) ) ;
#6360 = CARTESIAN_POINT ( 'NONE',  ( 0.7331010873566492503, 12.82195173545669320, -6.628039790227788330 ) ) ;
#6361 = CARTESIAN_POINT ( 'NONE',  ( -2.500000000000000000, 27.43419673618999965, 0.000000000000000000 ) ) ;
#6362 = CARTESIAN_POINT ( 'NONE',  ( -19.38578478962144302, -9.503017921997821915, 4.413944164837940498 ) ) ;
#6363 = CARTESIAN_POINT ( 'NONE',  ( 4.914858397426013603, 14.34199478478198841, 3.826882337439999393 ) ) ;
#6364 = CARTESIAN_POINT ( 'NONE',  ( -1.474515923050999655, 11.54597486106999504, -4.712210093417001922 ) ) ;
#6365 = ORIENTED_EDGE ( 'NONE', *, *, #20189, .F. ) ;
#6366 = CARTESIAN_POINT ( 'NONE',  ( -16.79120132807066312, 6.696678809309016600, -7.978545510531970919 ) ) ;
#6367 = DIRECTION ( 'NONE',  ( 0.000000000000000000, 1.000000000000000000, 0.000000000000000000 ) ) ;
#6368 = AXIS2_PLACEMENT_3D ( 'NONE', #22933, #777, #6351 ) ;
#6369 = CARTESIAN_POINT ( 'NONE',  ( -1.533592183623019967, 28.53112818204400725, 1.575162359379769006 ) ) ;
#6370 = DIRECTION ( 'NONE',  ( 1.000000000000000000, 0.000000000000000000, 0.000000000000000000 ) ) ;
#6371 = DIRECTION ( 'NONE',  ( -1.000000000000000000, 0.000000000000000000, 0.000000000000000000 ) ) ;
#6372 = VERTEX_POINT ( 'NONE', #5557 ) ;
#6373 = LINE ( 'NONE', #23075, #2218 ) ;
#6374 = CIRCLE ( 'NONE', #21076, 10.50000000000000000 ) ;
#6375 = CARTESIAN_POINT ( 'NONE',  ( 13.11693924931000055, 9.054732109491999026, 5.598051111924999823 ) ) ;
#6376 = CARTESIAN_POINT ( 'NONE',  ( -21.32896435853999861, -10.30805567071999995, 4.255407315586999140 ) ) ;
#6377 = CARTESIAN_POINT ( 'NONE',  ( -6.294047091888000267, 15.63810218524001172, 1.260373451110999188 ) ) ;
#6378 = CARTESIAN_POINT ( 'NONE',  ( 15.66749951745999958, 9.735035431332001110, -0.2247563725877999852 ) ) ;
#6379 = CARTESIAN_POINT ( 'NONE',  ( 0.000000000000000000, 21.95000012746600149, -2.704938617610999654E-14 ) ) ;
#6380 = DIRECTION ( 'NONE',  ( 0.000000000000000000, -0.8660254037844288266, 0.5000000000000169864 ) ) ;
#6381 = CARTESIAN_POINT ( 'NONE',  ( 24.65654608415999860, 9.344931615893999677, -2.926056642454999857 ) ) ;
#6382 = EDGE_CURVE ( 'NONE', #20600, #13895, #12934, .T. ) ;
#6383 = CARTESIAN_POINT ( 'NONE',  ( 23.99062354302999722, -7.716878364870000340, 11.63397459621999985 ) ) ;
#6384 = VERTEX_POINT ( 'NONE', #3519 ) ;
#6385 = CARTESIAN_POINT ( 'NONE',  ( 0.000000000000000000, 17.00000000000000000, 0.000000000000000000 ) ) ;
#6386 = CARTESIAN_POINT ( 'NONE',  ( 1.450871306011999984, 28.12913313894999945, 1.996953125041000199 ) ) ;
#6387 = VECTOR ( 'NONE', #4979, 1000.000000000000000 ) ;
#6388 = CARTESIAN_POINT ( 'NONE',  ( -0.1122646929101999980, 11.54752496335999012, 4.753533889266998713 ) ) ;
#6389 = CARTESIAN_POINT ( 'NONE',  ( 1.912977839466240892, 28.94241077574801579, 1.003607546239349890 ) ) ;
#6390 = CARTESIAN_POINT ( 'NONE',  ( -20.91269164496000244, 1.066062916854000120, -11.02412034271000074 ) ) ;
#6391 = FACE_OUTER_BOUND ( 'NONE', #14306, .T. ) ;
#6392 = EDGE_LOOP ( 'NONE', ( #5272, #19451, #4680, #16371 ) ) ;
#6393 = CARTESIAN_POINT ( 'NONE',  ( -24.11803009776757634, 4.367939700858217478, -12.49970390892939243 ) ) ;
#6394 = CARTESIAN_POINT ( 'NONE',  ( -1.254111594709508504, 11.63130255791515033, 4.623328579164538432 ) ) ;
#6395 = EDGE_CURVE ( 'NONE', #2137, #14425, #1687, .T. ) ;
#6396 = CARTESIAN_POINT ( 'NONE',  ( -3.693067381368000834, 13.86499636515999967, 4.815635213893004973 ) ) ;
#6397 = B_SPLINE_CURVE_WITH_KNOTS ( 'NONE', 3,
 ( #18163, #3387, #5310, #21549, #16431, #4964, #7004, #3265, #3610, #5085, #23709, #9176, #5197, #22017, #1565, #8951, #7115, #17917, #12349, #12699, #10993, #18379, #3150, #9060 ),
 .UNSPECIFIED., .F., .F.,
 ( 4, 2, 2, 2, 2, 2, 2, 2, 1, 1, 2, 2, 4 ),
 ( 0.000000000000000000, 0.2500000000000229816, 0.3750000000000345834, 0.4375000000000403011, 0.4687500000000402456, 0.5000000000000401901, 0.6250000000000424105, 0.6875000000000435207, 0.7187500000000440759, 0.7343750000000448530, 0.7421875000000460743, 0.7500000000000471845, 1.000000000000000000 ),
 .UNSPECIFIED. ) ;
#6398 = CARTESIAN_POINT ( 'NONE',  ( 0.9858775068236067529, 6.848474835707053288, 1.449525164644654751 ) ) ;
#6399 = DIRECTION ( 'NONE',  ( 1.000000000000000000, 0.000000000000000000, 0.000000000000000000 ) ) ;
#6400 = CARTESIAN_POINT ( 'NONE',  ( -6.159325028044951189, 15.88311956943892689, -1.090658714736985280 ) ) ;
#6401 = AXIS2_PLACEMENT_3D ( 'NONE', #2800, #10064, #20841 ) ;
#6402 = B_SPLINE_CURVE_WITH_KNOTS ( 'NONE', 3,
 ( #19870, #3286, #10668, #8491, #23619, #5219, #19987, #15857 ),
 .UNSPECIFIED., .F., .F.,
 ( 4, 2, 2, 4 ),
 ( 0.000000000000000000, 0.2499999999999997224, 0.4999999999999994449, 1.000000000000000000 ),
 .UNSPECIFIED. ) ;
#6403 = CARTESIAN_POINT ( 'NONE',  ( 15.23137625731000000, -4.902144360783999844, -7.754105707547999771 ) ) ;
#6404 = EDGE_CURVE ( 'NONE', #12389, #21355, #7967, .T. ) ;
#6405 = CARTESIAN_POINT ( 'NONE',  ( 24.36881528991199986, 3.090117214402293477, 12.50000000000000178 ) ) ;
#6406 = ORIENTED_EDGE ( 'NONE', *, *, #23877, .F. ) ;
#6407 = CARTESIAN_POINT ( 'NONE',  ( 20.62424770046331091, -7.357456981350354752, -5.654072255929076363 ) ) ;
#6408 = CARTESIAN_POINT ( 'NONE',  ( -0.3559997375695000410, 30.27669110727999779, -2.700474074450999851 ) ) ;
#6409 = DIRECTION ( 'NONE',  ( 0.000000000000000000, -1.000000000000000000, 0.000000000000000000 ) ) ;
#6410 = CARTESIAN_POINT ( 'NONE',  ( -2.357926041848682708, 13.96279335765504648, -5.653421260559023942 ) ) ;
#6411 = VERTEX_POINT ( 'NONE', #20685 ) ;
#6412 = DIRECTION ( 'NONE',  ( 0.000000000000000000, 1.000000000000000000, 0.000000000000000000 ) ) ;
#6413 = DIRECTION ( 'NONE',  ( 0.000000000000000000, -1.000000000000000000, 0.000000000000000000 ) ) ;
#6414 = EDGE_CURVE ( 'NONE', #19423, #16291, #8814, .T. ) ;
#6415 = CARTESIAN_POINT ( 'NONE',  ( -2.500000000000000000, 28.23419673618999681, 0.000000000000000000 ) ) ;
#6416 = CARTESIAN_POINT ( 'NONE',  ( 12.04708237236142487, -5.050716351111039337, 12.50004921246056355 ) ) ;
#6417 = CARTESIAN_POINT ( 'NONE',  ( -4.333208638113355882, 13.59008039607882345, 4.978090617012794539 ) ) ;
#6418 = CARTESIAN_POINT ( 'NONE',  ( -21.70078743917332886, -5.671049804393380356, -7.379548682649590852 ) ) ;
#6419 = CARTESIAN_POINT ( 'NONE',  ( 24.48327518124254354, -11.46871523476161059, -5.135602515852324856 ) ) ;
#6420 = EDGE_LOOP ( 'NONE', ( #20614, #1738, #7835, #6811 ) ) ;
#6421 = CARTESIAN_POINT ( 'NONE',  ( 0.000000000000000000, 28.15000000674550051, 0.000000000000000000 ) ) ;
#6422 = AXIS2_PLACEMENT_3D ( 'NONE', #7169, #6819, #12160 ) ;
#6423 = CARTESIAN_POINT ( 'NONE',  ( -4.749997084077000054, 12.55000000011000161, -4.491085162427999259E-09 ) ) ;
#6424 = ORIENTED_EDGE ( 'NONE', *, *, #9643, .F. ) ;
#6425 = DIRECTION ( 'NONE',  ( -1.000000000000000000, 0.000000000000000000, 0.000000000000000000 ) ) ;
#6426 = CARTESIAN_POINT ( 'NONE',  ( 0.7864549106799859635, 24.35740526346785018, -2.047056573199967033 ) ) ;
#6427 = EDGE_CURVE ( 'NONE', #13003, #23889, #17288, .T. ) ;
#6428 = CARTESIAN_POINT ( 'NONE',  ( 4.058888790243617706, 13.35463775849163426, 5.476079634781732430 ) ) ;
#6429 = CARTESIAN_POINT ( 'NONE',  ( 6.148088670540117207, 14.14458356372224834, -0.2229764228181548014 ) ) ;
#6430 = CARTESIAN_POINT ( 'NONE',  ( -6.418772728474004374, 15.32337082171999931, -1.206311712873000097 ) ) ;
#6431 = VECTOR ( 'NONE', #8778, 1000.000000000000114 ) ;
#6432 = FACE_OUTER_BOUND ( 'NONE', #11699, .T. ) ;
#6433 = EDGE_LOOP ( 'NONE', ( #6785, #9100, #15901, #17717, #21724, #5993 ) ) ;
#6434 = ORIENTED_EDGE ( 'NONE', *, *, #15129, .T. ) ;
#6435 = DIRECTION ( 'NONE',  ( -1.000000000000000000, 0.000000000000000000, 0.000000000000000000 ) ) ;
#6436 = CARTESIAN_POINT ( 'NONE',  ( -1.750000000000000000, 7.000000000000000000, -0.2229454749283412696 ) ) ;
#6437 = CARTESIAN_POINT ( 'NONE',  ( -20.18427425486666849, -9.189249971530744077, 1.048513845136502587 ) ) ;
#6438 = ORIENTED_EDGE ( 'NONE', *, *, #20801, .T. ) ;
#6439 = CARTESIAN_POINT ( 'NONE',  ( 4.000000000000000000, 28.30000000000000071, -2.309401076759000304 ) ) ;
#6440 = CONICAL_SURFACE ( 'NONE', #9536, 13.23032192316000000, 1.093540295016705466 ) ;
#6441 = CARTESIAN_POINT ( 'NONE',  ( 6.141065375610000210, 14.19649368052000149, -1.893142280157000292E-06 ) ) ;
#6442 = CARTESIAN_POINT ( 'NONE',  ( 15.22242881478463694, 5.018927266204900484, 9.044725437050461281 ) ) ;
#6443 = CARTESIAN_POINT ( 'NONE',  ( -17.29476926998999886, -4.783536645008999777, -9.995794592903001430 ) ) ;
#6444 = ADVANCED_FACE ( 'NONE', ( #17046 ), #10403, .F. ) ;
#6445 = CARTESIAN_POINT ( 'NONE',  ( 12.00000000000000000, -9.392874664203999302, -3.575135015595999999 ) ) ;
#6446 = CARTESIAN_POINT ( 'NONE',  ( -21.82254243295554375, 3.501655625743340661, 10.07467862742537967 ) ) ;
#6447 = EDGE_CURVE ( 'NONE', #3305, #11676, #11176, .T. ) ;
#6448 = DIRECTION ( 'NONE',  ( -0.000000000000000000, 1.000000000000000000, 0.000000000000000000 ) ) ;
#6449 = CARTESIAN_POINT ( 'NONE',  ( -1.485745231353044371, 29.50735104790518903, 1.567784488697564038 ) ) ;
#6450 = ORIENTED_EDGE ( 'NONE', *, *, #13348, .F. ) ;
#6451 = VECTOR ( 'NONE', #5275, 1000.000000000000000 ) ;
#6452 = CARTESIAN_POINT ( 'NONE',  ( -2.163129499999000060, 23.57098390934999799, -0.9155631307312001033 ) ) ;
#6453 = CARTESIAN_POINT ( 'NONE',  ( -15.41800740740231213, -1.436686530438418430, -10.28770811664919727 ) ) ;
#6454 = CIRCLE ( 'NONE', #3744, 10.65000000000000036 ) ;
#6455 = ORIENTED_EDGE ( 'NONE', *, *, #1737, .T. ) ;
#6456 = CARTESIAN_POINT ( 'NONE',  ( -24.50000000000000000, 1.524685264937999788E-14, 0.000000000000000000 ) ) ;
#6457 = CARTESIAN_POINT ( 'NONE',  ( 6.085566944076997942, 14.50612891015002326, -0.7765878609773998464 ) ) ;
#6458 = EDGE_CURVE ( 'NONE', #21807, #2989, #5791, .T. ) ;
#6459 = CARTESIAN_POINT ( 'NONE',  ( -4.820913734138907003, 13.23370548858168227, -5.762714020006541205 ) ) ;
#6460 = EDGE_CURVE ( 'NONE', #5053, #18160, #11725, .T. ) ;
#6461 = AXIS2_PLACEMENT_3D ( 'NONE', #15981, #23375, #21929 ) ;
#6462 = CARTESIAN_POINT ( 'NONE',  ( -20.18322087121332586, -5.647117051120087439, -7.348406657775178985 ) ) ;
#6463 = CARTESIAN_POINT ( 'NONE',  ( 14.49000142131000146, 7.205444258087999820, 6.439089808501999634 ) ) ;
#6464 = VERTEX_POINT ( 'NONE', #15338 ) ;
#6465 = CARTESIAN_POINT ( 'NONE',  ( 0.000000000000000000, 12.90000000000000036, 0.000000000000000000 ) ) ;
#6466 = DIRECTION ( 'NONE',  ( 1.000000000000000000, 0.000000000000000000, 0.000000000000000000 ) ) ;
#6467 = CARTESIAN_POINT ( 'NONE',  ( 2.818367767609802232, 24.55137445130672091, -2.991616928423186383 ) ) ;
#6468 = VERTEX_POINT ( 'NONE', #13174 ) ;
#6469 = CARTESIAN_POINT ( 'NONE',  ( 2.399999999999999911, 26.50000000000000355, 0.000000000000000000 ) ) ;
#6470 = CARTESIAN_POINT ( 'NONE',  ( -2.143277222256999792, 23.64327722226000006, 4.118360636503000477E-13 ) ) ;
#6471 = CARTESIAN_POINT ( 'NONE',  ( 4.811405344589000599, 12.64229255396000617, -0.1541548637438999170 ) ) ;
#6472 = CARTESIAN_POINT ( 'NONE',  ( -13.99999999999999822, -3.511891994211063572, 9.329532952517192612 ) ) ;
#6473 = CARTESIAN_POINT ( 'NONE',  ( 16.85684936900776876, 9.467955822817058831, 4.441589298551446241 ) ) ;
#6474 = CIRCLE ( 'NONE', #8008, 4.649999999999999467 ) ;
#6475 = LINE ( 'NONE', #11691, #13714 ) ;
#6476 = B_SPLINE_CURVE_WITH_KNOTS ( 'NONE', 3,
 ( #6287, #22751, #353, #11395, #13670 ),
 .UNSPECIFIED., .F., .F.,
 ( 4, 1, 4 ),
 ( 0.000000000000000000, 0.5000000000000000000, 1.000000000000000000 ),
 .UNSPECIFIED. ) ;
#6477 = CARTESIAN_POINT ( 'NONE',  ( -14.49999965082560038, -10.56569440617049693, 6.699684590240001292 ) ) ;
#6478 = CARTESIAN_POINT ( 'NONE',  ( 22.98768560147999906, -10.84767042793000158, -3.069029816253999954 ) ) ;
#6479 = AXIS2_PLACEMENT_3D ( 'NONE', #21157, #6251, #2876 ) ;
#6480 = CARTESIAN_POINT ( 'NONE',  ( 2.263491887170372419, 26.37901421991915640, -0.3060186196293296357 ) ) ;
#6481 = CARTESIAN_POINT ( 'NONE',  ( -4.396880683728629613, 13.55034449960124476, -5.013219078665608563 ) ) ;
#6482 = APPLICATION_CONTEXT ( 'automotive_design' ) ;
#6483 = DIRECTION ( 'NONE',  ( 0.000000000000000000, -0.9925668416490733836, 0.1217007183987965646 ) ) ;
#6484 = CIRCLE ( 'NONE', #4550, 15.45000000000000107 ) ;
#6485 = CARTESIAN_POINT ( 'NONE',  ( -2.148122869378203958, 30.19035462121604496, -0.2261009145559444433 ) ) ;
#6486 = ORIENTED_EDGE ( 'NONE', *, *, #11940, .F. ) ;
#6487 = CARTESIAN_POINT ( 'NONE',  ( -17.16578743917332872, 5.599530677400165857, 7.286485824131497147 ) ) ;
#6488 = CARTESIAN_POINT ( 'NONE',  ( 24.65994082994999914, -8.903700310608000379, -5.455873167974000459 ) ) ;
#6489 = CARTESIAN_POINT ( 'NONE',  ( 23.02309396335594371, -10.39063195256835392, 2.065499158806352042 ) ) ;
#6490 = CARTESIAN_POINT ( 'NONE',  ( 0.000000000000000000, -1.550000000000000044, 0.000000000000000000 ) ) ;
#6491 = CARTESIAN_POINT ( 'NONE',  ( -20.34973429036302761, 8.472421900539268691, -6.203803128982323223 ) ) ;
#6492 = DIRECTION ( 'NONE',  ( 0.000000000000000000, 0.000000000000000000, 1.000000000000000000 ) ) ;
#6493 = AXIS2_PLACEMENT_3D ( 'NONE', #16290, #8564, #17890 ) ;
#6494 = CIRCLE ( 'NONE', #4561, 2.948682383037074750 ) ;
#6495 = CARTESIAN_POINT ( 'NONE',  ( -3.292290159323002285, 11.90693939058999717, -3.664509819767999499 ) ) ;
#6496 = EDGE_LOOP ( 'NONE', ( #6701, #1599, #1659, #538, #12935 ) ) ;
#6497 = CARTESIAN_POINT ( 'NONE',  ( -15.39563946661559335, -7.162326101167759695, -7.704075600233069920 ) ) ;
#6498 = CARTESIAN_POINT ( 'NONE',  ( -24.12232999016000079, 1.520060141252000183E-14, 0.000000000000000000 ) ) ;
#6499 = CARTESIAN_POINT ( 'NONE',  ( 4.649999999999999467, 22.00000000000000000, 0.000000000000000000 ) ) ;
#6500 =( LENGTH_UNIT ( ) NAMED_UNIT ( * ) SI_UNIT ( .MILLI., .METRE. ) );
#6501 = CARTESIAN_POINT ( 'NONE',  ( 4.749999920006001020, 24.30000007999099765, 4.227385663729999829E-08 ) ) ;
#6502 = EDGE_LOOP ( 'NONE', ( #16852, #11827, #14915, #2493, #3081 ) ) ;
#6503 = FACE_OUTER_BOUND ( 'NONE', #3322, .T. ) ;
#6504 = CARTESIAN_POINT ( 'NONE',  ( -12.13322999603999897, 6.430159825535999296, -13.55186498671000095 ) ) ;
#6505 = CARTESIAN_POINT ( 'NONE',  ( -20.68661761865999793, 2.890438285933000451, -10.75281663302000013 ) ) ;
#6506 = CARTESIAN_POINT ( 'NONE',  ( 13.83937451745999958, 9.661954171790000601, -0.6968930456070000501 ) ) ;
#6507 = CARTESIAN_POINT ( 'NONE',  ( -12.50000000000000000, 1.377727649040999975E-14, 0.000000000000000000 ) ) ;
#6508 = AXIS2_PLACEMENT_3D ( 'NONE', #6787, #18403, #3291 ) ;
#6509 = DIRECTION ( 'NONE',  ( 1.000000000000000000, 0.000000000000000000, 0.000000000000000000 ) ) ;
#6510 = FACE_OUTER_BOUND ( 'NONE', #22420, .T. ) ;
#6511 = ORIENTED_EDGE ( 'NONE', *, *, #3738, .F. ) ;
#6512 = CARTESIAN_POINT ( 'NONE',  ( -2.591910195247867588, 14.01870539676982652, 5.551144025186765418 ) ) ;
#6513 = CARTESIAN_POINT ( 'NONE',  ( 0.1571687770951999963, 27.74706776952000098, -2.665093312283999705 ) ) ;
#6514 = CARTESIAN_POINT ( 'NONE',  ( -1.894626972038001789, 11.71448426407998689, 4.353454451108000889 ) ) ;
#6515 = CARTESIAN_POINT ( 'NONE',  ( -19.84899577250665104, -4.623430325997634149, -8.021972148549920689 ) ) ;
#6516 = CIRCLE ( 'NONE', #8462, 1.500000000000000000 ) ;
#6517 = CARTESIAN_POINT ( 'NONE',  ( -24.86702589508999850, -9.268724920833001590, -5.486562022343000500 ) ) ;
#6518 = DIRECTION ( 'NONE',  ( 4.064457104213683579E-11, -1.000000000000000000, 0.000000000000000000 ) ) ;
#6519 = AXIS2_PLACEMENT_3D ( 'NONE', #10273, #23218, #11933 ) ;
#6520 = ORIENTED_EDGE ( 'NONE', *, *, #6869, .F. ) ;
#6521 = CARTESIAN_POINT ( 'NONE',  ( 4.715134770518538687, 12.39891044673686871, -1.126757662178899722 ) ) ;
#6522 = DIRECTION ( 'NONE',  ( 0.000000000000000000, 0.9995435980848492719, 0.03020919607658151262 ) ) ;
#6523 = B_SPLINE_CURVE_WITH_KNOTS ( 'NONE', 3,
 ( #19408, #19156, #13584, #21345, #20980, #8268, #21097, #22783, #6319, #2822, #6199, #21226 ),
 .UNSPECIFIED., .F., .F.,
 ( 4, 2, 2, 2, 2, 4 ),
 ( 0.000000000000000000, 0.2500000000000285882, 0.3750000000000284217, 0.4375000000000150435, 0.5000000000000016653, 1.000000000000000000 ),
 .UNSPECIFIED. ) ;
#6524 = CIRCLE ( 'NONE', #15412, 3.000000000000000000 ) ;
#6525 = CARTESIAN_POINT ( 'NONE',  ( 0.4441971634758341003, 6.791582890693172558, 1.695532875298955355 ) ) ;
#6526 = FACE_OUTER_BOUND ( 'NONE', #11006, .T. ) ;
#6527 = EDGE_CURVE ( 'NONE', #8499, #15019, #9394, .T. ) ;
#6528 = DIRECTION ( 'NONE',  ( 0.000000000000000000, -1.000000000000000000, 1.177781335444000003E-14 ) ) ;
#6529 = DIRECTION ( 'NONE',  ( 0.000000000000000000, -1.000000000000000000, 0.000000000000000000 ) ) ;
#6530 = CARTESIAN_POINT ( 'NONE',  ( 16.87668875730999929, -8.405545991651999671, -3.781450583054000170 ) ) ;
#6531 = CARTESIAN_POINT ( 'NONE',  ( 18.93569518786017625, 2.254188637666244333, 10.18821787601618389 ) ) ;
#6532 = AXIS2_PLACEMENT_3D ( 'NONE', #10552, #18184, #19871 ) ;
#6533 = ORIENTED_EDGE ( 'NONE', *, *, #9983, .T. ) ;
#6534 = CARTESIAN_POINT ( 'NONE',  ( 5.254686582598590228, 13.86014107681422658, 4.146971818284736599 ) ) ;
#6535 = CARTESIAN_POINT ( 'NONE',  ( 2.507121665491000240, 29.97271731528999794, -0.3598210903258999838 ) ) ;
#6536 = CARTESIAN_POINT ( 'NONE',  ( -15.54074577250666955, 8.833969188127328565, 2.374193597558468927 ) ) ;
#6537 = CARTESIAN_POINT ( 'NONE',  ( -3.244655456173217711, 14.19450280349881588, -5.218741847022917213 ) ) ;
#6538 = PRESENTATION_LAYER_ASSIGNMENT (  '', '', ( #8873 ) ) ;
#6539 = DIRECTION ( 'NONE',  ( -1.000000000000000000, 0.000000000000000000, 0.000000000000000000 ) ) ;
#6540 = CARTESIAN_POINT ( 'NONE',  ( -23.97728971655646291, -13.40084515672999999, 1.788539470836744583 ) ) ;
#6541 = FACE_OUTER_BOUND ( 'NONE', #14528, .T. ) ;
#6542 = ADVANCED_FACE ( 'NONE', ( #20564 ), #813, .T. ) ;
#6543 = CARTESIAN_POINT ( 'NONE',  ( 0.2668645045036935337, 24.51773570851615602, -2.370970244263094440 ) ) ;
#6544 = CARTESIAN_POINT ( 'NONE',  ( 14.28063830469686479, 0.5579475798881706750, -10.34970908510135068 ) ) ;
#6545 = CARTESIAN_POINT ( 'NONE',  ( 0.000000000000000000, 7.100000000000000533, -1.499999999999985345 ) ) ;
#6546 = CARTESIAN_POINT ( 'NONE',  ( -2.999999956181000016, 17.90000004382000043, 2.609181505839000138E-08 ) ) ;
#6547 = CARTESIAN_POINT ( 'NONE',  ( 19.79283103379665931, 5.641139947076246663, 7.340215926192572127 ) ) ;
#6548 = ORIENTED_EDGE ( 'NONE', *, *, #4899, .F. ) ;
#6549 = CARTESIAN_POINT ( 'NONE',  ( -24.50000000000000355, -8.564163989839817859, -6.165454747490947796 ) ) ;
#6550 = CARTESIAN_POINT ( 'NONE',  ( 11.10357421855443860, -10.32596577201156585, 7.114843450789537727 ) ) ;
#6551 = EDGE_LOOP ( 'NONE', ( #18522, #9888, #18744, #21924 ) ) ;
#6552 = CONICAL_SURFACE ( 'NONE', #19334, 7.249999994833000727, 0.7853981633972997312 ) ;
#6553 = CARTESIAN_POINT ( 'NONE',  ( 0.6185100627188000466, 25.68299631853999898, 2.270477015093999906 ) ) ;
#6554 = CARTESIAN_POINT ( 'NONE',  ( -0.9242717917835999719, 23.66000000000000014, -1.952260652400999996 ) ) ;
#6555 = CARTESIAN_POINT ( 'NONE',  ( 0.000000000000000000, 26.35000000000000142, 0.000000000000000000 ) ) ;
#6556 = CARTESIAN_POINT ( 'NONE',  ( 6.155602479547902739, 14.09697471573797323, -0.3418480430767212863 ) ) ;
#6557 = FACE_OUTER_BOUND ( 'NONE', #18307, .T. ) ;
#6558 = EDGE_CURVE ( 'NONE', #8533, #10983, #12581, .T. ) ;
#6559 = CARTESIAN_POINT ( 'NONE',  ( 24.36881528991200341, -3.090117214402293921, -12.50000000000000178 ) ) ;
#6560 = B_SPLINE_CURVE_WITH_KNOTS ( 'NONE', 3,
 ( #14642, #3409, #16094, #1464, #8859, #3630 ),
 .UNSPECIFIED., .F., .F.,
 ( 4, 2, 4 ),
 ( 0.000000000000000000, 0.5000000000000000000, 1.000000000000000000 ),
 .UNSPECIFIED. ) ;
#6561 = VERTEX_POINT ( 'NONE', #18743 ) ;
#6562 = CARTESIAN_POINT ( 'NONE',  ( 0.000000000000000000, 20.05000017415440183, 0.000000000000000000 ) ) ;
#6563 = CARTESIAN_POINT ( 'NONE',  ( -0.6075102312704570018, 6.804820720190284611, -1.641503610285228065 ) ) ;
#6564 = CARTESIAN_POINT ( 'NONE',  ( 24.50000000000000000, 0.000000000000000000, 12.50000000000000000 ) ) ;
#6565 = ORIENTED_EDGE ( 'NONE', *, *, #18126, .F. ) ;
#6566 = CARTESIAN_POINT ( 'NONE',  ( -24.54599082030000190, -10.10573440607999984, 1.235225690210000060 ) ) ;
#6567 = FACE_OUTER_BOUND ( 'NONE', #587, .T. ) ;
#6568 = CARTESIAN_POINT ( 'NONE',  ( 20.41554166666666248, -5.650960392684353906, -7.352994588050344227 ) ) ;
#6569 = CARTESIAN_POINT ( 'NONE',  ( 15.23327592022675248, 4.680385583748051914, 9.218627023934693909 ) ) ;
#6570 = CARTESIAN_POINT ( 'NONE',  ( -14.37011451133999884, -7.634104718556999458, 7.921771262350999265 ) ) ;
#6571 = FACE_OUTER_BOUND ( 'NONE', #15737, .T. ) ;
#6572 = EDGE_CURVE ( 'NONE', #12128, #2115, #17355, .T. ) ;
#6573 = CARTESIAN_POINT ( 'NONE',  ( -22.26176253788000281, -9.242562415387000740, 0.000000000000000000 ) ) ;
#6574 = CARTESIAN_POINT ( 'NONE',  ( 4.741968828122999469, 12.61531461105000140, -0.1095802255754999566 ) ) ;
#6575 = FACE_OUTER_BOUND ( 'NONE', #182, .T. ) ;
#6576 = CARTESIAN_POINT ( 'NONE',  ( -1.679626819221629264, 29.31726910860015067, -1.358118087700189269 ) ) ;
#6577 = EDGE_LOOP ( 'NONE', ( #17366, #10756, #20977 ) ) ;
#6578 = CARTESIAN_POINT ( 'NONE',  ( -6.042815635770000249, 16.39253429789999927, 0.9999999720525000191 ) ) ;
#6579 = CARTESIAN_POINT ( 'NONE',  ( -14.69452806119251953, 7.308005346171998262, 7.484391584288502486 ) ) ;
#6580 = AXIS2_PLACEMENT_3D ( 'NONE', #6507, #6628, #810 ) ;
#6581 = EDGE_CURVE ( 'NONE', #7389, #1524, #17025, .T. ) ;
#6582 = ORIENTED_EDGE ( 'NONE', *, *, #3218, .F. ) ;
#6583 = DIRECTION ( 'NONE',  ( -1.000000000000000000, 0.000000000000000000, 0.000000000000000000 ) ) ;
#6584 = CARTESIAN_POINT ( 'NONE',  ( 5.996003309297000428, 13.65988289665999567, -2.867731330265999912 ) ) ;
#6585 = CARTESIAN_POINT ( 'NONE',  ( 12.00000000000000000, -7.193466889194404246, -5.390184783310134620 ) ) ;
#6586 = CARTESIAN_POINT ( 'NONE',  ( -12.25000000000000000, -13.75000000000000000, 0.000000000000000000 ) ) ;
#6587 = EDGE_CURVE ( 'NONE', #19976, #7164, #19039, .T. ) ;
#6588 = CARTESIAN_POINT ( 'NONE',  ( 18.75768908530999823, -5.059016186635999723, 8.765201904772998986 ) ) ;
#6589 = ADVANCED_FACE ( 'NONE', ( #19838 ), #20454, .T. ) ;
#6590 = VERTEX_POINT ( 'NONE', #1056 ) ;
#6591 = CARTESIAN_POINT ( 'NONE',  ( -4.549999999999999822, 22.00000000000000000, 0.000000000000000000 ) ) ;
#6592 = CARTESIAN_POINT ( 'NONE',  ( 2.184465970885645092, 26.86666666666667780, -1.259047450927249123 ) ) ;
#6593 = PRESENTATION_STYLE_ASSIGNMENT (( #23172 ) ) ;
#6594 = ORIENTED_EDGE ( 'NONE', *, *, #12899, .T. ) ;
#6595 = CARTESIAN_POINT ( 'NONE',  ( 11.09594815121266009, 10.32758188523873422, 7.112100880971675920 ) ) ;
#6596 = DIRECTION ( 'NONE',  ( 0.000000000000000000, 0.000000000000000000, -1.000000000000000000 ) ) ;
#6597 = PLANE ( 'NONE',  #13745 ) ;
#6598 = CARTESIAN_POINT ( 'NONE',  ( 16.97422162585966632, 6.903272406789144000, 7.796750432489865545 ) ) ;
#6599 = CARTESIAN_POINT ( 'NONE',  ( -24.00016455340000121, 1.715543117993999783E-14, 0.000000000000000000 ) ) ;
#6600 = CARTESIAN_POINT ( 'NONE',  ( -14.44097954155595431, 12.31212079859723296, -3.674767524707307054 ) ) ;
#6601 = EDGE_CURVE ( 'NONE', #17, #4069, #23370, .T. ) ;
#6602 = EDGE_CURVE ( 'NONE', #18727, #14183, #1720, .T. ) ;
#6603 = CARTESIAN_POINT ( 'NONE',  ( 6.243179582884000212, 13.63341776306000064, 1.952383140737000033 ) ) ;
#6604 = CARTESIAN_POINT ( 'NONE',  ( -23.74465998031000069, 7.716878364870000340, -11.63397459621999985 ) ) ;
#6605 = DIRECTION ( 'NONE',  ( 1.000000000000000000, 0.000000000000000000, 0.000000000000000000 ) ) ;
#6606 = CARTESIAN_POINT ( 'NONE',  ( -2.144556769453566769, 30.18852709384431066, -0.2572742967693883442 ) ) ;
#6607 = EDGE_LOOP ( 'NONE', ( #455, #7646, #6312, #6271 ) ) ;
#6608 = CARTESIAN_POINT ( 'NONE',  ( 19.12008073456999924, -10.59683341338999973, -2.226802362819999548 ) ) ;
#6609 = CARTESIAN_POINT ( 'NONE',  ( 23.36357456730870297, -5.878505771248656586, -8.824699706630454443 ) ) ;
#6610 = CARTESIAN_POINT ( 'NONE',  ( -6.250000000134000366, 16.31160393816000109, 2.000000000000000000 ) ) ;
#6611 = CARTESIAN_POINT ( 'NONE',  ( 0.5866479046345639548, 24.19681692063821288, -2.175561667358837603 ) ) ;
#6612 = CARTESIAN_POINT ( 'NONE',  ( 4.830312662056223338, 14.72996090241747069, 3.766125697359624880 ) ) ;
#6613 = FACE_OUTER_BOUND ( 'NONE', #15740, .T. ) ;
#6614 = ORIENTED_EDGE ( 'NONE', *, *, #15594, .F. ) ;
#6615 = CARTESIAN_POINT ( 'NONE',  ( -16.20506534625953776, 4.177158590315693587, 9.526121724279519754 ) ) ;
#6616 = PLANE ( 'NONE',  #282 ) ;
#6617 = CARTESIAN_POINT ( 'NONE',  ( -2.202320941319727776, 26.82989092620764993, 0.008350029242332654075 ) ) ;
#6618 = VECTOR ( 'NONE', #20265, 1000.000000000000114 ) ;
#6619 = CARTESIAN_POINT ( 'NONE',  ( 0.000000000000000000, 0.000000000000000000, 0.000000000000000000 ) ) ;
#6620 = CARTESIAN_POINT ( 'NONE',  ( -14.40719416829300670, -3.742543968318162051, -12.49988362782814022 ) ) ;
#6621 = EDGE_LOOP ( 'NONE', ( #20888, #21696, #13595, #7715 ) ) ;
#6622 = CARTESIAN_POINT ( 'NONE',  ( 2.500000000000000000, 26.80000000000000071, 0.000000000000000000 ) ) ;
#6623 = CARTESIAN_POINT ( 'NONE',  ( -4.069982105474159617, 15.01090283079260956, -4.577251214387113798 ) ) ;
#6624 = CARTESIAN_POINT ( 'NONE',  ( -20.04427087878999814, 6.764050733548000238, 8.822657572077998722 ) ) ;
#6625 = CARTESIAN_POINT ( 'NONE',  ( -18.26988800695000137, -1.530349862213000067, 10.77306797024999874 ) ) ;
#6626 = CARTESIAN_POINT ( 'NONE',  ( -5.982938424327000071, 16.41764137798000434, 1.007171089178999113 ) ) ;
#6627 = CARTESIAN_POINT ( 'NONE',  ( 15.05812451745999958, -5.188080995363999470, -8.220389579339999031 ) ) ;
#6628 = DIRECTION ( 'NONE',  ( -1.000000000000000000, 0.000000000000000000, 0.000000000000000000 ) ) ;
#6629 = CARTESIAN_POINT ( 'NONE',  ( -14.25622743459000041, 13.93375672974000068, 0.4334889134416999856 ) ) ;
#6630 = CARTESIAN_POINT ( 'NONE',  ( 24.15736593521593178, -8.253730364077119575, 10.70411965744399119 ) ) ;
#6631 = ORIENTED_EDGE ( 'NONE', *, *, #1771, .T. ) ;
#6632 = CARTESIAN_POINT ( 'NONE',  ( 2.724105571843130402, 14.05267863184722721, 5.486037458710886661 ) ) ;
#6633 = CARTESIAN_POINT ( 'NONE',  ( 0.9334375154566999511, 28.80369850838000190, 1.831974274068000064 ) ) ;
#6634 = CARTESIAN_POINT ( 'NONE',  ( -20.15132910583999859, -9.188404534074999574, 1.125025998286999896E-14 ) ) ;
#6635 = CARTESIAN_POINT ( 'NONE',  ( -21.07977619073999875, -5.139443787745999970, -9.816022020342002108 ) ) ;
#6636 = VERTEX_POINT ( 'NONE', #15824 ) ;
#6637 = DIRECTION ( 'NONE',  ( 0.000000000000000000, -1.000000000000000000, 0.000000000000000000 ) ) ;
#6638 = CARTESIAN_POINT ( 'NONE',  ( -23.74465998031000069, -6.216878364870000340, -12.50000000000000000 ) ) ;
#6639 = CARTESIAN_POINT ( 'NONE',  ( 0.7390662495429000112, 13.81263551691999503, 6.128930807943001824 ) ) ;
#6640 = DIRECTION ( 'NONE',  ( 0.000000000000000000, -1.000000000000000000, 0.000000000000000000 ) ) ;
#6641 = DIRECTION ( 'NONE',  ( -1.000000000000000000, 0.000000000000000000, 0.000000000000000000 ) ) ;
#6642 = CARTESIAN_POINT ( 'NONE',  ( -1.259047450927251788, 27.30086340285666680, -2.184465970885643316 ) ) ;
#6643 = CARTESIAN_POINT ( 'NONE',  ( 11.64686211521070724, -8.383335983967715066, -3.190882296136046570 ) ) ;
#6644 = CARTESIAN_POINT ( 'NONE',  ( 15.14812642130999976, -9.595485766438999420, 1.281252696419999948 ) ) ;
#6645 = CARTESIAN_POINT ( 'NONE',  ( 18.90322913654150483, 3.341522535781485281, 9.898536439817744892 ) ) ;
#6646 = AXIS2_PLACEMENT_3D ( 'NONE', #21257, #8050, #17131 ) ;
#6647 = ORIENTED_EDGE ( 'NONE', *, *, #912, .T. ) ;
#6648 = CARTESIAN_POINT ( 'NONE',  ( -1.536366799937290084, 28.68333333333333002, -1.999167105995448113 ) ) ;
#6649 = CARTESIAN_POINT ( 'NONE',  ( 1.997291889306999968, 30.03889703575999803, -1.557547871342000123 ) ) ;
#6650 = DIRECTION ( 'NONE',  ( 0.000000000000000000, 1.000000000000000000, 0.000000000000000000 ) ) ;
#6651 = CARTESIAN_POINT ( 'NONE',  ( -2.523824298054621718, 14.00207580638300264, -5.580858811804300323 ) ) ;
#6652 = ORIENTED_EDGE ( 'NONE', *, *, #15572, .F. ) ;
#6653 = CARTESIAN_POINT ( 'NONE',  ( 0.000000000000000000, 20.00000000000000000, 0.000000000000000000 ) ) ;
#6654 = CARTESIAN_POINT ( 'NONE',  ( -24.41513307469962513, -11.84921275889466763, 4.476505678113710474 ) ) ;
#6655 = B_SPLINE_SURFACE_WITH_KNOTS ( 'NONE', 3, 3, ( 
 ( #10847, #23783, #14354, #21745, #6962, #18457, #18340, #1750, #12540, #5158, #7189, #9137, #21973, #19928, #14806, #16151, #23670, #14698, #1867, #3346, #20046, #8789, #3463, #5388, #41, #10723, #21859, #9257, #18116, #1632, #9021, #12774, #1521, #8911, #16277 ),
 ( #20164, #7079, #16632, #16512, #14466, #7309, #5270, #22090, #5499, #12878, #3803, #12656, #20279, #7424, #22201, #5615, #12996, #11198, #1397, #18932, #15161, #626, #13347, #2099, #11433, #18806, #13590, #11670, #20747, #15401, #2454, #19044, #20987, #4399, #16993 ),
 ( #9488, #7911, #18581, #9845, #17227, #9606, #22557, #7545, #9727, #3924, #4154, #11550, #16864, #4282, #1984, #8028, #22791, #11316, #393, #16742, #6205, #20874, #20518, #2339, #5851, #14923, #15048, #9369, #17112, #153, #509, #22317, #5734, #13123, #18691 ),
 ( #6079, #267, #7672, #7791, #22441, #4038, #13236, #20627, #2215, #5962, #15277, #22669, #13470, #11911, #8637, #15521, #15999, #4647, #10465, #871, #15638, #14081, #17476, #21235, #22910, #23394, #23154, #15885, #2706, #19417, #21475, #10090, #19543, #8156, #4890 ) ),
 .UNSPECIFIED., .F., .F., .F.,
 ( 4, 4 ),
 ( 4, 1, 1, 1, 1, 1, 1, 1, 1, 1, 1, 1, 1, 1, 1, 1, 1, 1, 1, 1, 1, 1, 1, 1, 1, 1, 1, 1, 1, 1, 1, 1, 4 ),
 ( -0.08408083179840999954, 1.084080831798000188 ),
 ( -0.02000000000000000042, 0.01250000000000000069, 0.04499999999999999833, 0.07749999999999999944, 0.1100000000000000006, 0.1424999999999999878, 0.1749999999999999889, 0.2074999999999999900, 0.2399999999999999911, 0.2725000000000000200, 0.3049999999999999933, 0.3375000000000000222, 0.3699999999999999956, 0.4025000000000000244, 0.4349999999999999978, 0.4675000000000000266, 0.5000000000000000000, 0.5324999999999999734, 0.5649999999999999467, 0.5975000000000000311, 0.6300000000000000044, 0.6624999999999999778, 0.6949999999999999512, 0.7275000000000000355, 0.7600000000000000089, 0.7924999999999999822, 0.8249999999999999556, 0.8575000000000000400, 0.8900000000000000133, 0.9224999999999999867, 0.9549999999999999600, 0.9875000000000000444, 1.020000000000000018 ),
 .UNSPECIFIED. ) ;
#6656 = PLANE ( 'NONE',  #17734 ) ;
#6657 = CARTESIAN_POINT ( 'NONE',  ( -5.911109520797385386, 16.32704292856097439, 1.639614246112896856 ) ) ;
#6658 = CARTESIAN_POINT ( 'NONE',  ( 15.70237539785324365, -10.03438503088997891, -2.734757645857814889 ) ) ;
#6659 = CARTESIAN_POINT ( 'NONE',  ( -3.920367541008654477, 13.93676790526789411, 4.846056852944322202 ) ) ;
#6660 = DIRECTION ( 'NONE',  ( -1.000000000000000000, 0.000000000000000000, 0.000000000000000000 ) ) ;
#6661 = EDGE_CURVE ( 'NONE', #13113, #10909, #713, .T. ) ;
#6662 = CARTESIAN_POINT ( 'NONE',  ( 19.67945603379666153, 8.018170545278437089, 4.621239218893133049 ) ) ;
#6663 = VERTEX_POINT ( 'NONE', #15696 ) ;
#6664 = DIRECTION ( 'NONE',  ( 0.000000000000000000, -1.000000000000000000, 9.414779719719000361E-11 ) ) ;
#6665 = CARTESIAN_POINT ( 'NONE',  ( 11.12576011241401197, -10.20205618040264994, 7.329535452952375962 ) ) ;
#6666 = ORIENTED_EDGE ( 'NONE', *, *, #6010, .F. ) ;
#6667 = CARTESIAN_POINT ( 'NONE',  ( 2.241442604181999698, 25.09172815385999655, 1.205773825739000049 ) ) ;
#6668 = CARTESIAN_POINT ( 'NONE',  ( 5.929709434395003420, 14.11474726611999664, 1.364385784323000506 ) ) ;
#6669 = DIRECTION ( 'NONE',  ( 0.000000000000000000, 0.000000000000000000, 1.000000000000000000 ) ) ;
#6670 = CIRCLE ( 'NONE', #6281, 2.100000000000000089 ) ;
#6671 = FACE_OUTER_BOUND ( 'NONE', #14067, .T. ) ;
#6672 = CARTESIAN_POINT ( 'NONE',  ( -20.38485864507334000, -6.393576149522361085, 6.693947997704227326 ) ) ;
#6673 =( LENGTH_UNIT ( ) NAMED_UNIT ( * ) SI_UNIT ( .MILLI., .METRE. ) );
#6674 = EDGE_CURVE ( 'NONE', #11959, #6143, #23552, .T. ) ;
#6675 = VERTEX_POINT ( 'NONE', #21660 ) ;
#6676 = FACE_BOUND ( 'NONE', #10185, .T. ) ;
#6677 = CARTESIAN_POINT ( 'NONE',  ( 0.000000000000000000, 20.10000000000000142, 0.000000000000000000 ) ) ;
#6678 = CARTESIAN_POINT ( 'NONE',  ( -14.00000000000000000, 10.59999999999999964, 0.000000000000000000 ) ) ;
#6679 = ORIENTED_EDGE ( 'NONE', *, *, #16355, .T. ) ;
#6680 = CARTESIAN_POINT ( 'NONE',  ( -22.31822325740000323, -2.751304892524999879, -10.37736970521999957 ) ) ;
#6681 = CARTESIAN_POINT ( 'NONE',  ( 0.000000000000000000, 24.40000007355299871, 0.000000000000000000 ) ) ;
#6682 = CARTESIAN_POINT ( 'NONE',  ( 14.98414533422809036, 10.04427201105623446, 2.428330160207583965 ) ) ;
#6683 = CARTESIAN_POINT ( 'NONE',  ( 11.50000000000000000, 0.000000000000000000, 0.000000000000000000 ) ) ;
#6684 = CARTESIAN_POINT ( 'NONE',  ( 0.3498527751141999875, 29.44093971554000078, 2.330099399188000131 ) ) ;
#6685 = CARTESIAN_POINT ( 'NONE',  ( -22.41358485479884877, -8.081562438851669583, 4.657891738322038400 ) ) ;
#6686 = CARTESIAN_POINT ( 'NONE',  ( 0.3636138132592998673, 11.55177073541999277, -4.743661845547999079 ) ) ;
#6687 = EDGE_LOOP ( 'NONE', ( #19506, #7006, #16542, #6344, #21546, #12671 ) ) ;
#6688 = VECTOR ( 'NONE', #1354, 1000.000000000000000 ) ;
#6689 = DIRECTION ( 'NONE',  ( -1.000000000000000000, 0.000000000000000000, 0.000000000000000000 ) ) ;
#6690 = ADVANCED_FACE ( 'NONE', ( #23085 ), #13101, .T. ) ;
#6691 = CARTESIAN_POINT ( 'NONE',  ( -1.768277280319097811, 29.48163746745662905, 1.241304826943840256 ) ) ;
#6692 = ORIENTED_EDGE ( 'NONE', *, *, #13837, .T. ) ;
#6693 = CARTESIAN_POINT ( 'NONE',  ( -14.75240640888930521, 8.576432255687270967, 5.819130627761911256 ) ) ;
#6694 = EDGE_LOOP ( 'NONE', ( #20829, #22838, #1285, #2090 ) ) ;
#6695 = CARTESIAN_POINT ( 'NONE',  ( 2.500060036629733418, 30.00618913924456876, -0.1188157828604838595 ) ) ;
#6696 = CARTESIAN_POINT ( 'NONE',  ( 4.981589731873999227, 14.41790566382999650, -3.496892685228000008 ) ) ;
#6697 = CARTESIAN_POINT ( 'NONE',  ( 12.00000000000000000, -2.135184344106596299, -8.725065291608126827 ) ) ;
#6698 = CARTESIAN_POINT ( 'NONE',  ( 17.36604605622000008, -10.43477088592999813, 3.767700144398000273 ) ) ;
#6699 = ADVANCED_FACE ( 'NONE', ( #6510 ), #5753, .F. ) ;
#6700 = CARTESIAN_POINT ( 'NONE',  ( 13.52925158531000172, -9.668754250937999117, 3.079128054934999525 ) ) ;
#6701 = ORIENTED_EDGE ( 'NONE', *, *, #20189, .T. ) ;
#6702 = DIRECTION ( 'NONE',  ( -1.000000000000000000, 0.000000000000000000, 0.000000000000000000 ) ) ;
#6703 = LINE ( 'NONE', #21490, #22697 ) ;
#6704 = CARTESIAN_POINT ( 'NONE',  ( -2.399999988617999680, 29.99999998861800066, -6.349992589004001159E-08 ) ) ;
#6705 = ORIENTED_EDGE ( 'NONE', *, *, #66, .T. ) ;
#6706 = DIRECTION ( 'NONE',  ( 0.000000000000000000, 0.000000000000000000, 1.000000000000000000 ) ) ;
#6707 = CARTESIAN_POINT ( 'NONE',  ( 11.45478115325815160, 9.254429737878785645, 8.970723317470367775 ) ) ;
#6708 = CARTESIAN_POINT ( 'NONE',  ( 0.000000000000000000, 24.29999999999999716, 0.000000000000000000 ) ) ;
#6709 = CARTESIAN_POINT ( 'NONE',  ( -6.044090623820190800, 14.96394378892167509, -3.756777771135694000 ) ) ;
#6710 = CARTESIAN_POINT ( 'NONE',  ( 17.24009154054752457, -2.043749485021590928, 10.22276658632487667 ) ) ;
#6711 = AXIS2_PLACEMENT_3D ( 'NONE', #11063, #9247, #19918 ) ;
#6712 = EDGE_CURVE ( 'NONE', #20551, #12102, #2664, .T. ) ;
#6713 = CARTESIAN_POINT ( 'NONE',  ( -18.63966243917333898, -4.608035645285467830, 7.994758007891237028 ) ) ;
#6714 = CARTESIAN_POINT ( 'NONE',  ( -14.45960639177118701, 12.05326364612464829, -4.123067891182894407 ) ) ;
#6715 = CARTESIAN_POINT ( 'NONE',  ( 1.099193499486128101, 26.43562577624027199, 3.984182490697167900 ) ) ;
#6716 = DIRECTION ( 'NONE',  ( 0.000000000000000000, -1.000000000000000000, 0.000000000000000000 ) ) ;
#6717 = EDGE_CURVE ( 'NONE', #2989, #15509, #2884, .T. ) ;
#6718 = CARTESIAN_POINT ( 'NONE',  ( -2.159896986047187273, 30.20407674326398251, 0.006713223370198041426 ) ) ;
#6719 = VERTEX_POINT ( 'NONE', #18485 ) ;
#6720 = ADVANCED_FACE ( 'NONE', ( #16420 ), #2257, .T. ) ;
#6721 = CARTESIAN_POINT ( 'NONE',  ( 0.6085180536320998756, 25.64793633493999891, 2.255015312327000032 ) ) ;
#6722 = CARTESIAN_POINT ( 'NONE',  ( 22.01884473796000208, 7.419280916948000737, 7.996861738661001695 ) ) ;
#6723 = CARTESIAN_POINT ( 'NONE',  ( 22.90960042870581148, -8.796780507069112076, 5.889649883977557288 ) ) ;
#6724 = CARTESIAN_POINT ( 'NONE',  ( 1.536366799937295413, 27.71753006952333465, 1.999167105995444338 ) ) ;
#6725 = ORIENTED_EDGE ( 'NONE', *, *, #18144, .T. ) ;
#6726 = DIRECTION ( 'NONE',  ( 0.000000000000000000, -1.000000000000000000, 0.000000000000000000 ) ) ;
#6727 = CARTESIAN_POINT ( 'NONE',  ( -2.099999992529999915, 28.30000000747030242, -4.159306751197999787E-08 ) ) ;
#6728 = CARTESIAN_POINT ( 'NONE',  ( 3.268619611001000624, 11.96755932734001782, -3.750657828938995575 ) ) ;
#6729 = ORIENTED_EDGE ( 'NONE', *, *, #2740, .F. ) ;
#6730 = CARTESIAN_POINT ( 'NONE',  ( -15.11652709432294905, 2.218820346475768090, -10.13318491115196984 ) ) ;
#6731 = ADVANCED_FACE ( 'NONE', ( #21887 ), #3064, .T. ) ;
#6732 = DIRECTION ( 'NONE',  ( 0.000000000000000000, 1.000000000000000000, 0.000000000000000000 ) ) ;
#6733 = ORIENTED_EDGE ( 'NONE', *, *, #12772, .F. ) ;
#6734 = CARTESIAN_POINT ( 'NONE',  ( 1.633102778084561724, 27.13808608125045296, 1.430956311882127352 ) ) ;
#6735 = CARTESIAN_POINT ( 'NONE',  ( 60.61494135913342518, 37.01856778792605240, 0.000000000000000000 ) ) ;
#6736 = ORIENTED_EDGE ( 'NONE', *, *, #7310, .F. ) ;
#6737 = CARTESIAN_POINT ( 'NONE',  ( 21.91677564524432853, 36.61664399928019265, 6.000000000000000000 ) ) ;
#6738 = CARTESIAN_POINT ( 'NONE',  ( -12.15500686398999797, 12.23011958036999935, -9.372058967585999767 ) ) ;
#6739 = CARTESIAN_POINT ( 'NONE',  ( -23.41659126313000172, -2.571795304491000245, 10.90924587281000058 ) ) ;
#6740 = CARTESIAN_POINT ( 'NONE',  ( -19.14845983621999892, 9.556232533099999316, -4.027326457250000047 ) ) ;
#6741 = CARTESIAN_POINT ( 'NONE',  ( -6.019884510648998877, 15.84348053695000580, 1.061877742816000225 ) ) ;
#6742 = CARTESIAN_POINT ( 'NONE',  ( 15.19306994526000132, 7.671504830348000681, -6.819139572487000756 ) ) ;
#6743 = CARTESIAN_POINT ( 'NONE',  ( -4.000000000000000000, 26.20000000000000284, -2.309401076759000304 ) ) ;
#6744 = CARTESIAN_POINT ( 'NONE',  ( 20.05326942813999835, -8.291560945558000384, 4.969461368340999385 ) ) ;
#6745 = EDGE_CURVE ( 'NONE', #6273, #3203, #4903, .T. ) ;
#6746 = CARTESIAN_POINT ( 'NONE',  ( 24.40278699097224546, -9.495349905928280876, 8.553571527287482823 ) ) ;
#6747 = EDGE_LOOP ( 'NONE', ( #10766, #18000, #11645, #5979 ) ) ;
#6748 = EDGE_CURVE ( 'NONE', #6244, #19945, #12704, .T. ) ;
#6749 = AXIS2_PLACEMENT_3D ( 'NONE', #19557, #10596, #15651 ) ;
#6750 = CARTESIAN_POINT ( 'NONE',  ( -17.57559587121334488, 7.970898357189208028, 4.594283802594034682 ) ) ;
#6751 = CARTESIAN_POINT ( 'NONE',  ( -3.644446339697000159, 14.33206891720999998, 4.922772686299000000 ) ) ;
#6752 = CARTESIAN_POINT ( 'NONE',  ( -0.3106091461881000382, 27.92619850838000062, 2.245636445400999825 ) ) ;
#6753 = B_SPLINE_CURVE_WITH_KNOTS ( 'NONE', 3,
 ( #11883, #20963, #6301, #2926, #847, #3052, #17323, #10438, #19136, #8613, #4620, #9937, #970, #10309, #1098, #8498, #12011, #6423 ),
 .UNSPECIFIED., .F., .F.,
 ( 4, 2, 2, 2, 2, 2, 2, 2, 4 ),
 ( 0.000000000000000000, 0.1250000000000000000, 0.2500000000000000000, 0.3750000000000000000, 0.5000000000000000000, 0.6250000000000000000, 0.7500000000000000000, 0.8750000000000000000, 1.000000000000000000 ),
 .UNSPECIFIED. ) ;
#6754 = CARTESIAN_POINT ( 'NONE',  ( -19.43328743917331636, 7.333017253390695878, -5.635290240896845937 ) ) ;
#6755 = CARTESIAN_POINT ( 'NONE',  ( -23.92021346900000012, 8.712087150140002123, 6.970052773374000310 ) ) ;
#6756 = AXIS2_PLACEMENT_3D ( 'NONE', #14462, #1273, #19809 ) ;
#6757 = CARTESIAN_POINT ( 'NONE',  ( -3.058559774358916350, 11.87684768202457342, 3.734032921821529794 ) ) ;
#6758 = VERTEX_POINT ( 'NONE', #18872 ) ;
#6759 = DIRECTION ( 'NONE',  ( 1.000000000000000000, 0.000000000000000000, 0.000000000000000000 ) ) ;
#6760 = CARTESIAN_POINT ( 'NONE',  ( 4.713500436508303970, 12.39829890550265290, -1.133475946671276491 ) ) ;
#6761 = EDGE_CURVE ( 'NONE', #23793, #20574, #8102, .T. ) ;
#6762 = CARTESIAN_POINT ( 'NONE',  ( 24.01519597621253510, -6.071732368389049839, -7.117487303104867102 ) ) ;
#6763 = ADVANCED_FACE ( 'NONE', ( #16930 ), #332, .F. ) ;
#6764 = AXIS2_PLACEMENT_3D ( 'NONE', #14108, #21269, #4677 ) ;
#6765 = CARTESIAN_POINT ( 'NONE',  ( -20.82567920454666677, -2.409692318855363169, 8.966061123404951871 ) ) ;
#6766 = FACE_OUTER_BOUND ( 'NONE', #4863, .T. ) ;
#6767 = CARTESIAN_POINT ( 'NONE',  ( -18.72408206190999991, 5.159378177076999528, -10.19862909758999869 ) ) ;
#6768 = CARTESIAN_POINT ( 'NONE',  ( 15.91593892131000132, 7.924234377949000319, -5.595770532261999719 ) ) ;
#6769 = CARTESIAN_POINT ( 'NONE',  ( 24.38510397947347741, 2.890284505278650773, 12.50000000000000000 ) ) ;
#6770 = ORIENTED_EDGE ( 'NONE', *, *, #6838, .T. ) ;
#6771 = CARTESIAN_POINT ( 'NONE',  ( -22.38043928506862557, -1.210159647712697240, 9.247744296678623854 ) ) ;
#6772 = CARTESIAN_POINT ( 'NONE',  ( 0.4178678117584000429, 29.87961278443000168, 2.691594793395000185 ) ) ;
#6773 = CARTESIAN_POINT ( 'NONE',  ( -14.78491243917333442, -8.815175007119801620, 2.368882121629280579 ) ) ;
#6774 = CARTESIAN_POINT ( 'NONE',  ( -0.5814258234044360485, 13.67896451797541779, -6.147206943646843946 ) ) ;
#6775 = AXIS2_PLACEMENT_3D ( 'NONE', #9191, #2038, #9428 ) ;
#6776 = ORIENTED_EDGE ( 'NONE', *, *, #5912, .F. ) ;
#6777 = CARTESIAN_POINT ( 'NONE',  ( -1.067140290979515571, 26.49999999999999645, -2.247699653298786515 ) ) ;
#6778 = CARTESIAN_POINT ( 'NONE',  ( -24.36724102302310158, 12.10481948367283422, -4.033677606666548066 ) ) ;
#6779 = CARTESIAN_POINT ( 'NONE',  ( 6.038532390086429835, 14.39630362418530751, 1.042615058007298812 ) ) ;
#6780 = CARTESIAN_POINT ( 'NONE',  ( -4.724999999999999645, 13.10000000000000142, 0.000000000000000000 ) ) ;
#6781 = CARTESIAN_POINT ( 'NONE',  ( 16.39930534548422614, 9.330189097337756365, -4.632983890435689034 ) ) ;
#6782 = LINE ( 'NONE', #19759, #4472 ) ;
#6783 = CARTESIAN_POINT ( 'NONE',  ( -4.371713857110997026, 12.30683965646000999, 2.325230957305000068 ) ) ;
#6784 = CARTESIAN_POINT ( 'NONE',  ( 20.13295603379664911, -4.627100187415565280, 8.028339412451956036 ) ) ;
#6785 = ORIENTED_EDGE ( 'NONE', *, *, #21266, .F. ) ;
#6786 = DIRECTION ( 'NONE',  ( -1.000000000000000000, 0.000000000000000000, 0.000000000000000000 ) ) ;
#6787 = CARTESIAN_POINT ( 'NONE',  ( -10.90000000000000036, 7.200000000000000178, 4.317524282537999640E-09 ) ) ;
#6788 = ORIENTED_EDGE ( 'NONE', *, *, #22244, .T. ) ;
#6789 = CARTESIAN_POINT ( 'NONE',  ( -2.203461932915999899, 24.77914110727999741, -1.623795195417000015 ) ) ;
#6790 = CARTESIAN_POINT ( 'NONE',  ( 0.000000000000000000, 24.49999999999999645, 0.000000000000000000 ) ) ;
#6791 = FACE_OUTER_BOUND ( 'NONE', #20218, .T. ) ;
#6792 = AXIS2_PLACEMENT_3D ( 'NONE', #20804, #7965, #17286 ) ;
#6793 = CARTESIAN_POINT ( 'NONE',  ( 19.41266666666667007, 7.735111250169313557, 5.102936606934582286 ) ) ;
#6794 = CARTESIAN_POINT ( 'NONE',  ( -0.3272492347489393549, 27.81666666666668064, -2.499999999999999556 ) ) ;
#6795 = FACE_OUTER_BOUND ( 'NONE', #15404, .T. ) ;
#6796 = ORIENTED_EDGE ( 'NONE', *, *, #6601, .F. ) ;
#6797 = CARTESIAN_POINT ( 'NONE',  ( -2.184465970885641983, 29.90086340285667177, 1.259047450927253564 ) ) ;
#6798 = B_SPLINE_CURVE_WITH_KNOTS ( 'NONE', 3,
 ( #2369, #5883, #15077, #13382, #22706, #20783, #6240, #17394, #22826, #13622 ),
 .UNSPECIFIED., .F., .F.,
 ( 4, 1, 1, 2, 2, 4 ),
 ( 0.000000000000000000, 0.2499999999999994449, 0.3749999999999994449, 0.4375000000000000000, 0.5000000000000005551, 1.000000000000000000 ),
 .UNSPECIFIED. ) ;
#6799 = DIRECTION ( 'NONE',  ( 1.000000000000000000, 0.000000000000000000, 0.000000000000000000 ) ) ;
#6800 = DIRECTION ( 'NONE',  ( 0.000000000000000000, -1.000000000000000000, 0.000000000000000000 ) ) ;
#6801 = EDGE_CURVE ( 'NONE', #22764, #12346, #13537, .T. ) ;
#6802 = EDGE_LOOP ( 'NONE', ( #14759, #4803, #13221, #16409, #7587, #6365 ) ) ;
#6803 = CARTESIAN_POINT ( 'NONE',  ( -23.41894536462999810, 0.9629491129631000401, 11.24764485372000067 ) ) ;
#6804 = DIRECTION ( 'NONE',  ( 6.552635476078902493E-07, -0.9999999999997853939, -1.009232707941984266E-09 ) ) ;
#6805 = CARTESIAN_POINT ( 'NONE',  ( 15.00664151501544374, 9.822743592524254552, 3.215862093219099105 ) ) ;
#6806 = CARTESIAN_POINT ( 'NONE',  ( 3.999702431745993270, 24.50639765414744531, 0.3779811684581091957 ) ) ;
#6807 = AXIS2_PLACEMENT_3D ( 'NONE', #21967, #3457, #1861 ) ;
#6808 = CARTESIAN_POINT ( 'NONE',  ( -2.167698761436000154, 29.29258811475999735, 0.03558365842844000287 ) ) ;
#6809 = CARTESIAN_POINT ( 'NONE',  ( -18.69965283593333538, -8.970713245661908530, 2.088197045339661884 ) ) ;
#6810 = CARTESIAN_POINT ( 'NONE',  ( 4.614156076205000012, 12.49299253157998635, -1.062903411340000437 ) ) ;
#6811 = ORIENTED_EDGE ( 'NONE', *, *, #9715, .T. ) ;
#6812 = AXIS2_PLACEMENT_3D ( 'NONE', #9265, #15170, #9378 ) ;
#6813 = DIRECTION ( 'NONE',  ( 1.000000000000000000, 0.000000000000000000, 0.000000000000000000 ) ) ;
#6814 = CARTESIAN_POINT ( 'NONE',  ( -0.8021525768333287454, 29.25217003084671674, -2.005518083782086514 ) ) ;
#6815 = ORIENTED_EDGE ( 'NONE', *, *, #17844, .T. ) ;
#6816 = DIRECTION ( 'NONE',  ( 1.000000000000000000, 0.000000000000000000, 0.000000000000000000 ) ) ;
#6817 = CARTESIAN_POINT ( 'NONE',  ( -14.83922393043447308, 9.919015930220274058, 3.020892133029422943 ) ) ;
#6818 = EDGE_LOOP ( 'NONE', ( #18981, #5487, #2518, #10269 ) ) ;
#6819 = DIRECTION ( 'NONE',  ( 0.000000000000000000, 0.000000000000000000, 1.000000000000000000 ) ) ;
#6820 = CARTESIAN_POINT ( 'NONE',  ( 11.36701043059983718, -12.20499207204286840, -3.860262462454134624 ) ) ;
#6821 = CARTESIAN_POINT ( 'NONE',  ( 12.00000000000000000, -1.827539693554861788, -8.792163972483878709 ) ) ;
#6822 = CARTESIAN_POINT ( 'NONE',  ( 18.84348253994000189, -5.598984228891000114, 8.803251650347998947 ) ) ;
#6823 = CARTESIAN_POINT ( 'NONE',  ( 13.85831408531000086, -6.842896344163999167, -7.504413997217999288 ) ) ;
#6824 = EDGE_LOOP ( 'NONE', ( #20240, #6679, #5712, #11672, #15964, #15144 ) ) ;
#6825 = CARTESIAN_POINT ( 'NONE',  ( -10.82554149291999934, -14.29998144107999991, -2.504234213954000143 ) ) ;
#6826 = CIRCLE ( 'NONE', #18063, 0.09999999999999939493 ) ;
#6827 = DIRECTION ( 'NONE',  ( 0.000000000000000000, -1.000000000000000000, 0.000000000000000000 ) ) ;
#6828 =( NAMED_UNIT ( * ) PLANE_ANGLE_UNIT ( ) SI_UNIT ( $, .RADIAN. ) );
#6829 = EDGE_CURVE ( 'NONE', #5826, #4476, #579, .T. ) ;
#6830 = ORIENTED_EDGE ( 'NONE', *, *, #464, .F. ) ;
#6831 =( LENGTH_UNIT ( ) NAMED_UNIT ( * ) SI_UNIT ( .MILLI., .METRE. ) );
#6832 = CARTESIAN_POINT ( 'NONE',  ( 11.10357421856110705, 11.32461805837391822, 5.385126951717674082 ) ) ;
#6833 = CARTESIAN_POINT ( 'NONE',  ( 21.55864741212693758, 1.361786730296197678, -10.62933302226472065 ) ) ;
#6834 = CARTESIAN_POINT ( 'NONE',  ( -14.00000000000000178, 8.277532166501742950, 3.835819509332607513 ) ) ;
#6835 = CARTESIAN_POINT ( 'NONE',  ( 16.20461591949403513, -2.540617249209156103, -10.04820973369444914 ) ) ;
#6836 = CARTESIAN_POINT ( 'NONE',  ( -6.249999999916000526, 15.09564573669999987, 3.212813967733000098 ) ) ;
#6837 = DIRECTION ( 'NONE',  ( 0.000000000000000000, 1.000000000000000000, 0.000000000000000000 ) ) ;
#6838 = EDGE_CURVE ( 'NONE', #12555, #7943, #19690, .T. ) ;
#6839 = CARTESIAN_POINT ( 'NONE',  ( -1.215228304390323144, 30.08000406326414478, -1.785700434939019532 ) ) ;
#6840 = ORIENTED_EDGE ( 'NONE', *, *, #9240, .T. ) ;
#6841 = CARTESIAN_POINT ( 'NONE',  ( 1.694552266659000050, 25.71773410043999775, 1.607489577807000192 ) ) ;
#6842 = CARTESIAN_POINT ( 'NONE',  ( 11.18529249866647213, 11.69879683432484541, -4.737131156255078857 ) ) ;
#6843 = CARTESIAN_POINT ( 'NONE',  ( -2.326721815211127023E-16, 9.000000000000000000, 1.899912543625706274 ) ) ;
#6844 = CONICAL_SURFACE ( 'NONE', #1442, 13.23032192316000000, 1.235249617460683957 ) ;
#6845 = CYLINDRICAL_SURFACE ( 'NONE', #4116, 2.500000000000000000 ) ;
#6846 = ORIENTED_EDGE ( 'NONE', *, *, #7007, .T. ) ;
#6847 = CARTESIAN_POINT ( 'NONE',  ( 24.28455689590255773, -8.829963675777257492, -9.706054284564595847 ) ) ;
#6848 = CARTESIAN_POINT ( 'NONE',  ( 4.861474503319399787, 14.51472929299590753, 3.787796979831960176 ) ) ;
#6849 = CARTESIAN_POINT ( 'NONE',  ( -18.63376253787999914, -9.149460784975000038, 0.000000000000000000 ) ) ;
#6850 = ORIENTED_EDGE ( 'NONE', *, *, #4912, .T. ) ;
#6851 = CARTESIAN_POINT ( 'NONE',  ( 18.26606375730999687, -4.551782674040000032, 7.886397731525000232 ) ) ;
#6852 = ORIENTED_EDGE ( 'NONE', *, *, #12229, .F. ) ;
#6853 = CIRCLE ( 'NONE', #20787, 9.574826156038998448 ) ;
#6854 = CARTESIAN_POINT ( 'NONE',  ( 8.124934037954998800, 0.000000000000000000, 0.000000000000000000 ) ) ;
#6855 = PRODUCT_CONTEXT ( 'NONE', #8034, 'mechanical' ) ;
#6856 = DIRECTION ( 'NONE',  ( -0.5000000000000169864, 0.000000000000000000, -0.8660254037844289376 ) ) ;
#6857 = EDGE_CURVE ( 'NONE', #15294, #12632, #18244, .T. ) ;
#6858 = ORIENTED_EDGE ( 'NONE', *, *, #4623, .T. ) ;
#6859 = VECTOR ( 'NONE', #16434, 1000.000000000000000 ) ;
#6860 = CARTESIAN_POINT ( 'NONE',  ( -18.86729207711333345, -6.366495818929248429, 6.665594812321431917 ) ) ;
#6861 = CARTESIAN_POINT ( 'NONE',  ( -12.36677000395999926, 13.67685060524999940, -6.159850446377999056 ) ) ;
#6862 = CARTESIAN_POINT ( 'NONE',  ( -22.07990519880999969, 5.007857226526000183, 9.402496424037000367 ) ) ;
#6863 = CIRCLE ( 'NONE', #11371, 2.949999999999999734 ) ;
#6864 = CARTESIAN_POINT ( 'NONE',  ( -17.11715635651999889, 9.674678649335000102, 3.573597797309999713 ) ) ;
#6865 = CARTESIAN_POINT ( 'NONE',  ( 0.000000000000000000, 24.80000000000000426, 4.618802153517000519 ) ) ;
#6866 = CARTESIAN_POINT ( 'NONE',  ( 17.69874951746000136, 7.302264014228000200, 6.527174038894000496 ) ) ;
#6867 = CARTESIAN_POINT ( 'NONE',  ( 2.064425410739836764, 26.64466069140416593, -0.6742583458788029560 ) ) ;
#6868 = CARTESIAN_POINT ( 'NONE',  ( 12.00000000000000000, 0.000000000000000000, 0.000000000000000000 ) ) ;
#6869 = EDGE_CURVE ( 'NONE', #23810, #15717, #10400, .T. ) ;
#6870 = DIRECTION ( 'NONE',  ( 0.000000000000000000, 1.000000000000000000, 0.000000000000000000 ) ) ;
#6871 = EDGE_LOOP ( 'NONE', ( #9259, #6922, #10095, #8467 ) ) ;
#6872 = CARTESIAN_POINT ( 'NONE',  ( 23.29781751312559379, 8.206174485158717502, 4.349602372406548234 ) ) ;
#6873 = CARTESIAN_POINT ( 'NONE',  ( 1.483509881833009691, 13.79912375866350338, 5.942645371621392947 ) ) ;
#6874 = CARTESIAN_POINT ( 'NONE',  ( -2.214344957515000267, 26.17119850838000161, 0.4858445502740000310 ) ) ;
#6875 = VECTOR ( 'NONE', #5403, 1000.000000000000000 ) ;
#6876 = CARTESIAN_POINT ( 'NONE',  ( -24.75563619790999681, -6.749210113364999764, -8.912303601106998485 ) ) ;
#6877 = B_SPLINE_CURVE_WITH_KNOTS ( 'NONE', 3,
 ( #7045, #5121, #8875, #20005 ),
 .UNSPECIFIED., .F., .F.,
 ( 4, 4 ),
 ( 0.000000000000000000, 1.000000000000000000 ),
 .UNSPECIFIED. ) ;
#6878 = CARTESIAN_POINT ( 'NONE',  ( -1.495637945045119599, 11.56875457997782775, 4.606283421593187377 ) ) ;
#6879 = ORIENTED_EDGE ( 'NONE', *, *, #22555, .F. ) ;
#6880 = CARTESIAN_POINT ( 'NONE',  ( 22.24928936712999672, -9.242242329243000043, 0.000000000000000000 ) ) ;
#6881 = CARTESIAN_POINT ( 'NONE',  ( 3.757891690360106285, 12.07210435675419369, -3.048890984311763308 ) ) ;
#6882 = DIRECTION ( 'NONE',  ( 0.9996708941621509359, -0.02565352539214875091, -2.545944944692875236E-14 ) ) ;
#6883 = CARTESIAN_POINT ( 'NONE',  ( -20.44776253787999920, -9.196011600180998613, 0.000000000000000000 ) ) ;
#6884 = VERTEX_POINT ( 'NONE', #3014 ) ;
#6885 = ADVANCED_FACE ( 'NONE', ( #15945 ), #17794, .F. ) ;
#6886 = EDGE_CURVE ( 'NONE', #4269, #8374, #23162, .T. ) ;
#6887 = LINE ( 'NONE', #23604, #6859 ) ;
#6888 = CARTESIAN_POINT ( 'NONE',  ( -6.082217688135330924, 16.10188874983086649, -1.020520473285583485 ) ) ;
#6889 = VECTOR ( 'NONE', #21789, 1000.000000000000114 ) ;
#6890 = CARTESIAN_POINT ( 'NONE',  ( 13.50281392131000047, -8.671483154093998280, -4.205333541112000084 ) ) ;
#6891 = CARTESIAN_POINT ( 'NONE',  ( 18.76830727444978208, 7.489704376429600963, 7.283379905210109584 ) ) ;
#6892 = ORIENTED_EDGE ( 'NONE', *, *, #2453, .F. ) ;
#6893 = CARTESIAN_POINT ( 'NONE',  ( 5.155714003469999973, 13.97328511022999997, 4.008150528822999270 ) ) ;
#6894 = CARTESIAN_POINT ( 'NONE',  ( 2.135264558818000147, 30.59525960993000027, 0.9615570694947999097 ) ) ;
#6895 = PLANE ( 'NONE',  #14932 ) ;
#6896 = CARTESIAN_POINT ( 'NONE',  ( 13.49999999999999645, -7.667152171304032038, 6.546859119036191998 ) ) ;
#6897 = EDGE_LOOP ( 'NONE', ( #14042, #18703, #5594, #23800 ) ) ;
#6899 = VECTOR ( 'NONE', #1896, 1000.000000000000000 ) ;
#6898 = CARTESIAN_POINT ( 'NONE',  ( -7.500000000000000000, 24.99999999999999645, -6.000000000000000000 ) ) ;
#6900 = CARTESIAN_POINT ( 'NONE',  ( -24.43506354683005100, -11.72249354572810986, 4.696109227415885989 ) ) ;
#6901 = DIRECTION ( 'NONE',  ( 0.000000000000000000, -1.000000000000000000, 0.000000000000000000 ) ) ;
#6902 = ADVANCED_FACE ( 'NONE', ( #15830 ), #8081, .T. ) ;
#6903 = CARTESIAN_POINT ( 'NONE',  ( -5.554207712812456954, 16.15574578901152947, 2.609433215957428942 ) ) ;
#6904 = EDGE_CURVE ( 'NONE', #5348, #3528, #8701, .T. ) ;
#6905 = CARTESIAN_POINT ( 'NONE',  ( 16.14841056433666822, 2.481077197559224512, -10.10691008888976938 ) ) ;
#6906 = FACE_OUTER_BOUND ( 'NONE', #7453, .T. ) ;
#6907 = CONICAL_SURFACE ( 'NONE', #17338, 2.949999944334000368, 0.7853981633972997312 ) ;
#6908 = CARTESIAN_POINT ( 'NONE',  ( 4.540657248691003289, 12.36579710560998002, 1.969985720665999640 ) ) ;
#6909 = CARTESIAN_POINT ( 'NONE',  ( 20.24633103379666821, -7.349522212044369951, 5.648291859775539159 ) ) ;
#6910 = ORIENTED_EDGE ( 'NONE', *, *, #8942, .T. ) ;
#6911 = CARTESIAN_POINT ( 'NONE',  ( 2.309807618587000011, 30.69019238141000017, -7.292675330123999428E-08 ) ) ;
#6912 = DIRECTION ( 'NONE',  ( 0.000000000000000000, 1.792956356299999973E-10, -1.000000000000000000 ) ) ;
#6913 = AXIS2_PLACEMENT_3D ( 'NONE', #15138, #606, #11769 ) ;
#6914 = ORIENTED_EDGE ( 'NONE', *, *, #15154, .F. ) ;
#6915 = CARTESIAN_POINT ( 'NONE',  ( 0.6691735853424000124, 24.29144915060000187, 2.654084007310999915 ) ) ;
#6916 = CARTESIAN_POINT ( 'NONE',  ( 5.994133932293998157, 14.09831428825999744, 1.046105555905998408 ) ) ;
#6917 = CARTESIAN_POINT ( 'NONE',  ( 12.04708237234661183, 5.050716351078905042, -12.50004921245747802 ) ) ;
#6918 = CARTESIAN_POINT ( 'NONE',  ( 6.187913781813814573, 13.93138848470324831, -0.7590350555155512824 ) ) ;
#6919 = CARTESIAN_POINT ( 'NONE',  ( 13.49999999999999822, -2.699842513522783261, 10.00691734096826480 ) ) ;
#6920 = AXIS2_PLACEMENT_3D ( 'NONE', #13317, #22881, #360 ) ;
#6921 =( NAMED_UNIT ( * ) PLANE_ANGLE_UNIT ( ) SI_UNIT ( $, .RADIAN. ) );
#6922 = ORIENTED_EDGE ( 'NONE', *, *, #28, .F. ) ;
#6923 = CARTESIAN_POINT ( 'NONE',  ( 0.000000000000000000, 22.00000000000000000, 0.000000000000000000 ) ) ;
#6924 = AXIS2_PLACEMENT_3D ( 'NONE', #10749, #19950, #7337 ) ;
#6925 = PLANE ( 'NONE',  #16719 ) ;
#6926 = CARTESIAN_POINT ( 'NONE',  ( -4.000024251878889991, 24.52555747447230416, 0.7498250608958048069 ) ) ;
#6927 = ORIENTED_EDGE ( 'NONE', *, *, #13514, .F. ) ;
#6928 = CARTESIAN_POINT ( 'NONE',  ( -23.86052387786999773, 6.793182627230999415, -8.367515183292999481 ) ) ;
#6929 = DIRECTION ( 'NONE',  ( 0.000000000000000000, -1.000000000000000000, 0.000000000000000000 ) ) ;
#6930 = CARTESIAN_POINT ( 'NONE',  ( 14.89101776721218684, 10.28666262955564825, -0.9606185904953363774 ) ) ;
#6931 = VECTOR ( 'NONE', #8000, 1000.000000000000000 ) ;
#6932 = CARTESIAN_POINT ( 'NONE',  ( 4.000000142207500886, 24.55137445130360518, 0.9449696197344532589 ) ) ;
#6933 = CARTESIAN_POINT ( 'NONE',  ( 20.60157508292000017, 1.509805238461999988, 11.10580479464999826 ) ) ;
#6934 = CARTESIAN_POINT ( 'NONE',  ( 0.4664974798648000021, 28.71811702996999927, 2.117149378852999586 ) ) ;
#6935 = CARTESIAN_POINT ( 'NONE',  ( 13.59973893363859609, 6.904209829052242675, -5.804544132843785675 ) ) ;
#6936 = CARTESIAN_POINT ( 'NONE',  ( -4.447662105364998730, 12.42909450830998352, -1.606648311090999481 ) ) ;
#6937 = ORIENTED_EDGE ( 'NONE', *, *, #21569, .F. ) ;
#6938 = CARTESIAN_POINT ( 'NONE',  ( -21.84605420454664326, -1.208325219156637376, -9.231894520236238577 ) ) ;
#6939 = CIRCLE ( 'NONE', #6532, 4.750000000000000000 ) ;
#6940 = ORIENTED_EDGE ( 'NONE', *, *, #18141, .F. ) ;
#6941 = DIRECTION ( 'NONE',  ( 1.000000000000000000, 0.000000000000000000, 0.000000000000000000 ) ) ;
#6942 = CARTESIAN_POINT ( 'NONE',  ( 19.75000000000000000, -1.659811535170000019, 9.026773995975998943 ) ) ;
#6943 = AXIS2_PLACEMENT_3D ( 'NONE', #13240, #17453, #9610 ) ;
#6944 = VECTOR ( 'NONE', #20872, 1000.000000000000000 ) ;
#6945 = ORIENTED_EDGE ( 'NONE', *, *, #20286, .T. ) ;
#6946 = CARTESIAN_POINT ( 'NONE',  ( 0.9911964488588560496, 30.15065117088173707, -2.420280545933024552 ) ) ;
#6947 = CARTESIAN_POINT ( 'NONE',  ( 11.22285964979241690, -9.825076113722889914, -7.982449282815227143 ) ) ;
#6948 = CARTESIAN_POINT ( 'NONE',  ( 24.50000000000000000, 0.000000000000000000, 0.000000000000000000 ) ) ;
#6949 = AXIS2_PLACEMENT_3D ( 'NONE', #22446, #17116, #22562 ) ;
#6950 = CARTESIAN_POINT ( 'NONE',  ( 17.58032625501999746, -6.868895417556999838, -8.719434656480000712 ) ) ;
#6951 = EDGE_LOOP ( 'NONE', ( #16374, #20619, #12309 ) ) ;
#6952 = CARTESIAN_POINT ( 'NONE',  ( -11.23283149291999905, -0.5530958232186000689, 14.50705838281999860 ) ) ;
#6953 = CARTESIAN_POINT ( 'NONE',  ( 13.50000000000000000, 6.526939024554766711, 7.647570657964006813 ) ) ;
#6954 = AXIS2_PLACEMENT_3D ( 'NONE', #8074, #544, #6120 ) ;
#6955 = ORIENTED_EDGE ( 'NONE', *, *, #15839, .F. ) ;
#6956 = CARTESIAN_POINT ( 'NONE',  ( 11.06619116163223282, 10.57612823871844654, 6.681605107870990601 ) ) ;
#6957 = CARTESIAN_POINT ( 'NONE',  ( 21.08801403234133787, -10.51584647305647735, -0.7453109682132889047 ) ) ;
#6958 = CARTESIAN_POINT ( 'NONE',  ( 1.699986466736000068, 9.100024030970999434, -1.053574575520999757 ) ) ;
#6959 = CARTESIAN_POINT ( 'NONE',  ( 16.27412929406614950, -0.09366976407831074936, -10.36545759699181168 ) ) ;
#6960 = CARTESIAN_POINT ( 'NONE',  ( -18.86641243917333099, 2.396297420769109454, 8.917188256816995562 ) ) ;
#6961 = CARTESIAN_POINT ( 'NONE',  ( 1.566978647078999920, 29.92110055533999713, -1.741866172968000059 ) ) ;
#6962 = CARTESIAN_POINT ( 'NONE',  ( -18.19554712229000160, -2.285746783449999597, -9.537972663088998715 ) ) ;
#6963 = CARTESIAN_POINT ( 'NONE',  ( -0.5809343010167346000, 30.03825264969940179, -2.087773477905597641 ) ) ;
#6964 = ORIENTED_EDGE ( 'NONE', *, *, #19487, .T. ) ;
#6965 = CARTESIAN_POINT ( 'NONE',  ( 23.34331150348194228, -0.6078572885738241505, 9.272076336171188871 ) ) ;
#6966 = CARTESIAN_POINT ( 'NONE',  ( 11.10357421854642013, 10.32596577204267518, -7.114843450730285568 ) ) ;
#6967 = CARTESIAN_POINT ( 'NONE',  ( 22.82448027771794585, -6.707976417501984479, 8.192708876736357837 ) ) ;
#6968 = CARTESIAN_POINT ( 'NONE',  ( -10.34021276376999943, 7.200000000000000178, 5.302004252305999846E-09 ) ) ;
#6969 = B_SPLINE_CURVE_WITH_KNOTS ( 'NONE', 3,
 ( #13390, #7352, #11357, #20791, #80, #11241, #14848, #3846, #16906, #310, #9885, #12079 ),
 .UNSPECIFIED., .F., .F.,
 ( 4, 1, 1, 1, 1, 2, 2, 4 ),
 ( 0.000000000000000000, 0.2500000000000006106, 0.3750000000000012768, 0.4375000000000013323, 0.4687500000000012768, 0.4843750000000014433, 0.5000000000000016653, 1.000000000000000000 ),
 .UNSPECIFIED. ) ;
#6970 = EDGE_LOOP ( 'NONE', ( #739, #19055, #11218, #16402 ) ) ;
#6971 = EDGE_CURVE ( 'NONE', #8904, #19391, #23137, .T. ) ;
#6972 = CARTESIAN_POINT ( 'NONE',  ( -1.042632460611140788, 24.73976796275902146, 1.891962004173780576 ) ) ;
#6973 = CARTESIAN_POINT ( 'NONE',  ( -6.000000000000000000, 24.99999999999999645, 1.000000000000000000 ) ) ;
#6974 = CARTESIAN_POINT ( 'NONE',  ( -4.009361469255999566, 12.11895015699999689, -2.855765722793998762 ) ) ;
#6975 = VERTEX_POINT ( 'NONE', #19318 ) ;
#6976 = DIRECTION ( 'NONE',  ( 1.000000000000000000, 0.000000000000000000, 0.000000000000000000 ) ) ;
#6977 = EDGE_LOOP ( 'NONE', ( #18583, #5276, #19226, #767 ) ) ;
#6978 = CARTESIAN_POINT ( 'NONE',  ( -2.649999999999999911, 26.50000000000000000, 0.000000000000000000 ) ) ;
#6979 = SHAPE_DEFINITION_REPRESENTATION ( #8253, #22521 ) ;
#6980 = DIRECTION ( 'NONE',  ( 0.000000000000000000, -1.000000000000000000, 0.000000000000000000 ) ) ;
#6981 = EDGE_CURVE ( 'NONE', #10557, #20353, #775, .T. ) ;
#6982 = ORIENTED_EDGE ( 'NONE', *, *, #21465, .F. ) ;
#6983 = CARTESIAN_POINT ( 'NONE',  ( -19.17035378445833871, 2.613855109476041161, 8.847292803866498190 ) ) ;
#6984 = CARTESIAN_POINT ( 'NONE',  ( -4.690941914108488930, 15.65021434981036741, -3.939840772426298265 ) ) ;
#6985 = CARTESIAN_POINT ( 'NONE',  ( -25.02553073364999747, -3.263946373367999865, -9.309921254180999028 ) ) ;
#6986 = CARTESIAN_POINT ( 'NONE',  ( -18.19885853377000373, -7.619903537905999613, -6.175610338995999982 ) ) ;
#6987 = CARTESIAN_POINT ( 'NONE',  ( 22.35132670216743023, 35.07441746931982607, -115.0195023120000002 ) ) ;
#6988 = CARTESIAN_POINT ( 'NONE',  ( -23.90708761851598751, 10.11530264397083556, 3.143216488129493058 ) ) ;
#6989 = CARTESIAN_POINT ( 'NONE',  ( 1.805717673759776210, 27.47944697561501570, -1.207647802767778167 ) ) ;
#6990 = LINE ( 'NONE', #12209, #3101 ) ;
#6991 = CARTESIAN_POINT ( 'NONE',  ( 2.146186176612843610, 30.61809763272861318, -0.2430268685427999509 ) ) ;
#6992 = ORIENTED_EDGE ( 'NONE', *, *, #5925, .F. ) ;
#6993 = DIRECTION ( 'NONE',  ( -1.000000000000000000, 0.000000000000000000, 0.000000000000000000 ) ) ;
#6994 = B_SPLINE_CURVE_WITH_KNOTS ( 'NONE', 3,
 ( #10193, #22651, #13693, #21087, #11653, #15746, #17584, #17459, #853, #23012, #6429, #13814, #19524, #21213, #6556, #13941, #21335, #4751, #9708, #6060, #19024, #17947, #3179, #10317, #6918, #21457, #12729, #18067, #10681, #14063, #5229, #3057, #12259, #23631, #23740, #21585, #12614, #18195, #17708, #1105, #19647, #17833, #14314, #4999, #7036, #1475, #8869 ),
 .UNSPECIFIED., .F., .F.,
 ( 4, 2, 1, 1, 2, 2, 2, 1, 1, 1, 2, 2, 2, 2, 1, 1, 2, 2, 2, 1, 1, 1, 1, 2, 2, 2, 2, 2, 4 ),
 ( 0.000000000000000000, 0.06249999999999583666, 0.09374999999999411582, 0.1093749999999932415, 0.1171874999999927419, 0.1249999999999922562, 0.1874999999999966138, 0.2187499999999982236, 0.2343749999999995837, 0.2421875000000003331, 0.2460937500000001665, 0.2500000000000000000, 0.3750000000000012768, 0.4375000000000019429, 0.4687500000000022760, 0.4843750000000019984, 0.4921875000000016098, 0.5000000000000013323, 0.6249999999999892308, 0.6874999999999834577, 0.7187499999999802380, 0.7343749999999787947, 0.7421874999999783507, 0.7460937499999782396, 0.7499999999999782396, 0.8124999999999840128, 0.8437499999999866773, 0.8749999999999892308, 1.000000000000000000 ),
 .UNSPECIFIED. ) ;
#6995 = CARTESIAN_POINT ( 'NONE',  ( -2.411020654974999733, 26.27663313894999675, 0.5289967318968999965 ) ) ;
#6996 = EDGE_CURVE ( 'NONE', #14445, #709, #12718, .T. ) ;
#6997 = CARTESIAN_POINT ( 'NONE',  ( 5.575791046645279359, 14.52390015031493320, -2.648501204029414247 ) ) ;
#6998 = CARTESIAN_POINT ( 'NONE',  ( -1.862634475845999837, 26.92437716036000239, -1.590840130251000017 ) ) ;
#6999 = AXIS2_PLACEMENT_3D ( 'NONE', #19997, #1472, #17831 ) ;
#7000 = CARTESIAN_POINT ( 'NONE',  ( -3.280903357640863049, 11.93481450532642540, 3.545272627676774313 ) ) ;
#7001 = ORIENTED_EDGE ( 'NONE', *, *, #18501, .T. ) ;
#7002 = FACE_BOUND ( 'NONE', #14793, .T. ) ;
#7003 = CARTESIAN_POINT ( 'NONE',  ( 4.559109341211414979, 12.34130269922110834, -1.643108070882763450 ) ) ;
#7004 = CARTESIAN_POINT ( 'NONE',  ( -10.26377187911747768, 15.76328787329322623, 1.163182374018775889 ) ) ;
#7005 = CARTESIAN_POINT ( 'NONE',  ( 11.47028936713000036, -8.379193606113998882, -3.189305674207999708 ) ) ;
#7006 = ORIENTED_EDGE ( 'NONE', *, *, #6886, .T. ) ;
#7007 = EDGE_CURVE ( 'NONE', #18186, #13296, #8465, .T. ) ;
#7008 = CARTESIAN_POINT ( 'NONE',  ( -1.978156802582415441, 30.64141917833904927, -1.302609384799360503 ) ) ;
#7009 = DIRECTION ( 'NONE',  ( 0.000000000000000000, 1.000000000000000000, 0.000000000000000000 ) ) ;
#7010 = CARTESIAN_POINT ( 'NONE',  ( 13.39312642131000075, -9.609817522467999140, -0.6894128909195000876 ) ) ;
#7011 = CARTESIAN_POINT ( 'NONE',  ( 18.46047941552955862, 9.997012766731819156, -2.944153169368156409 ) ) ;
#7012 = VERTEX_POINT ( 'NONE', #17012 ) ;
#7013 = LINE ( 'NONE', #5661, #4215 ) ;
#7014 = CARTESIAN_POINT ( 'NONE',  ( 1.417687315775000068, 28.83533196750000016, 1.617399067864000006 ) ) ;
#7015 = DIRECTION ( 'NONE',  ( 0.000000000000000000, -0.7071067811866525998, -0.7071067811864425456 ) ) ;
#7016 = CARTESIAN_POINT ( 'NONE',  ( 13.50000000000000178, -5.635803601607234370, 8.567832869351823533 ) ) ;
#7017 = EDGE_LOOP ( 'NONE', ( #5836, #2576, #19183, #15290 ) ) ;
#7018 = EDGE_CURVE ( 'NONE', #15471, #20328, #11033, .T. ) ;
#7019 = LINE ( 'NONE', #18051, #6387 ) ;
#7020 = CARTESIAN_POINT ( 'NONE',  ( 0.000000000000000000, 22.10000000618969906, -2.849999993810000021 ) ) ;
#7021 = DIRECTION ( 'NONE',  ( 0.000000000000000000, 1.000000000000000000, 0.000000000000000000 ) ) ;
#7022 = CARTESIAN_POINT ( 'NONE',  ( -23.81628036379132141, -7.177005027323463793, 6.439087892836417026 ) ) ;
#7023 = CARTESIAN_POINT ( 'NONE',  ( 0.000000000000000000, 26.50000000000000355, 0.000000000000000000 ) ) ;
#7024 = DIRECTION ( 'NONE',  ( 0.000000000000000000, 1.000000000000000000, 0.000000000000000000 ) ) ;
#7025 = CARTESIAN_POINT ( 'NONE',  ( -4.940775639143002884, 12.51284741021001246, -0.1550196392192998707 ) ) ;
#7026 = EDGE_CURVE ( 'NONE', #2748, #4269, #9564, .T. ) ;
#7027 = CARTESIAN_POINT ( 'NONE',  ( 3.000000000000000000, 22.00000000000000000, 0.000000000000000000 ) ) ;
#7028 = EDGE_LOOP ( 'NONE', ( #21028, #20962 ) ) ;
#7029 = DIRECTION ( 'NONE',  ( 0.000000000000000000, -1.000000000000000000, 0.000000000000000000 ) ) ;
#7030 = ADVANCED_FACE ( 'NONE', ( #8052 ), #23809, .F. ) ;
#7031 = FACE_OUTER_BOUND ( 'NONE', #5511, .T. ) ;
#7032 = ORIENTED_EDGE ( 'NONE', *, *, #8463, .F. ) ;
#7033 = CARTESIAN_POINT ( 'NONE',  ( -2.496851939000000353, 25.57942011053999920, 0.4936453752708000464 ) ) ;
#7034 = CARTESIAN_POINT ( 'NONE',  ( 6.081738458038996598, 14.07685609792998527, -0.03589047288854997630 ) ) ;
#7035 = CARTESIAN_POINT ( 'NONE',  ( 11.40904387244272655, -2.948332260696405971, -12.49995270680654613 ) ) ;
#7036 = CARTESIAN_POINT ( 'NONE',  ( 6.242375959467782565, 13.66332201415649372, -1.753597398281198094 ) ) ;
#7037 = CARTESIAN_POINT ( 'NONE',  ( 0.000000000000000000, 20.04999987253367877, -4.699999872533999756 ) ) ;
#7038 = B_SPLINE_CURVE_WITH_KNOTS ( 'NONE', 3,
 ( #18738, #17283, #7725, #7839, #20800, #4210, #10144, #13760, #8574, #4820, #17900, #1181, #23328, #1051, #3133, #19595, #21162, #8207 ),
 .UNSPECIFIED., .F., .F.,
 ( 4, 2, 2, 2, 2, 2, 2, 2, 4 ),
 ( 0.000000000000000000, 0.1249999999999999445, 0.2499999999999998890, 0.3749999999999999445, 0.5000000000000000000, 0.6250000000000000000, 0.7500000000000001110, 0.8750000000000000000, 1.000000000000000000 ),
 .UNSPECIFIED. ) ;
#7039 = AXIS2_PLACEMENT_3D ( 'NONE', #4175, #11687, #15181 ) ;
#7040 = CARTESIAN_POINT ( 'NONE',  ( -12.24999999459000044, 1.554281285377000029E-14, -7.249999994590990759 ) ) ;
#7041 = EDGE_CURVE ( 'NONE', #379, #3901, #411, .T. ) ;
#7042 = EDGE_LOOP ( 'NONE', ( #18790, #5621, #785, #14124, #12737, #1816, #3476 ) ) ;
#7043 = CARTESIAN_POINT ( 'NONE',  ( -18.23630520352000062, 4.669879042777999700, -9.230749285618999878 ) ) ;
#7044 = DIRECTION ( 'NONE',  ( 0.000000000000000000, 0.000000000000000000, -1.000000000000000000 ) ) ;
#7045 = CARTESIAN_POINT ( 'NONE',  ( 1.699986747157999911, 9.000014340785000400, 0.8485215224771999187 ) ) ;
#7046 = EDGE_LOOP ( 'NONE', ( #5057, #8725, #19166, #4771 ) ) ;
#7047 = CARTESIAN_POINT ( 'NONE',  ( -22.14685652178999931, 3.522049787583000136, -10.13679110321000110 ) ) ;
#7048 = CARTESIAN_POINT ( 'NONE',  ( 0.8298323553694000321, 23.83132231056999828, 2.182665959441000059 ) ) ;
#7049 = CARTESIAN_POINT ( 'NONE',  ( 14.77010906259511458, 9.035887590412290393, -5.000320054086365040 ) ) ;
#7050 = AXIS2_PLACEMENT_3D ( 'NONE', #22628, #3886, #19000 ) ;
#7051 = FACE_OUTER_BOUND ( 'NONE', #12119, .T. ) ;
#7052 = CARTESIAN_POINT ( 'NONE',  ( 22.65751704163000113, -10.54215396955000017, 3.968579886229999687 ) ) ;
#7053 = CARTESIAN_POINT ( 'NONE',  ( 1.399243530816999925, 29.57982365715999862, 1.655989627749000048 ) ) ;
#7054 = CARTESIAN_POINT ( 'NONE',  ( 13.60043579687980220, 6.918659888968194949, -5.787303501411981799 ) ) ;
#7055 = CARTESIAN_POINT ( 'NONE',  ( -6.483873887681529169, 15.48026478585757459, -1.444101027390730208 ) ) ;
#7056 = CARTESIAN_POINT ( 'NONE',  ( -21.65709587121331836, 4.647032519295968278, -8.062418161751203627 ) ) ;
#7057 = VERTEX_POINT ( 'NONE', #9866 ) ;
#7058 = FACE_OUTER_BOUND ( 'NONE', #15339, .T. ) ;
#7059 = CIRCLE ( 'NONE', #19043, 2.000000000000000000 ) ;
#7060 = DIRECTION ( 'NONE',  ( 0.000000000000000000, -1.000000000000000000, 0.000000000000000000 ) ) ;
#7061 = B_SPLINE_CURVE_WITH_KNOTS ( 'NONE', 3,
 ( #6181, #13568, #20961, #21576, #3288 ),
 .UNSPECIFIED., .F., .F.,
 ( 4, 1, 4 ),
 ( 0.4999999999411116058, 0.6666666666667000474, 1.000000000000000000 ),
 .UNSPECIFIED. ) ;
#7062 = VERTEX_POINT ( 'NONE', #20893 ) ;
#7063 = CARTESIAN_POINT ( 'NONE',  ( 17.16545833333331217, 5.599525487243289135, -7.286479070541918901 ) ) ;
#7064 = CARTESIAN_POINT ( 'NONE',  ( 21.60683103379665226, 5.669747597873476153, 7.377441069599709245 ) ) ;
#7065 = CARTESIAN_POINT ( 'NONE',  ( 18.62920234113000006, 7.029629189252000643, 8.627757148559000555 ) ) ;
#7066 = EDGE_CURVE ( 'NONE', #8104, #20493, #4177, .T. ) ;
#7067 = ORIENTED_EDGE ( 'NONE', *, *, #5491, .F. ) ;
#7068 = EDGE_CURVE ( 'NONE', #10512, #5826, #11064, .T. ) ;
#7069 = CARTESIAN_POINT ( 'NONE',  ( -9.189007565846001313, -0.05028646118644999885, -14.86791649126999992 ) ) ;
#7070 = CARTESIAN_POINT ( 'NONE',  ( 13.50000000000000000, 9.554725887819582653, 1.841566180535791020 ) ) ;
#7071 = CARTESIAN_POINT ( 'NONE',  ( 1.350644574821315613, 28.02555747447238588, -3.839035148326051861 ) ) ;
#7072 = ORIENTED_EDGE ( 'NONE', *, *, #15668, .T. ) ;
#7073 = FILL_AREA_STYLE_COLOUR ( '', #10404 ) ;
#7074 = CARTESIAN_POINT ( 'NONE',  ( 21.79396410202163992, 8.711539071920352484, -6.251501696449420997 ) ) ;
#7075 = CARTESIAN_POINT ( 'NONE',  ( -2.900806500513820829, 26.43562577624027199, 2.944020739578862234 ) ) ;
#7076 = CARTESIAN_POINT ( 'NONE',  ( 16.01296168114131646, -8.180747814225620473, -6.354282860866971028 ) ) ;
#7077 = CARTESIAN_POINT ( 'NONE',  ( -19.16874577250666789, 8.924647632302601608, 2.398562752349402416 ) ) ;
#7078 = CARTESIAN_POINT ( 'NONE',  ( 0.3650451777216000004, 30.01137937871000005, -2.157632473909999682 ) ) ;
#7079 = CARTESIAN_POINT ( 'NONE',  ( -18.98111647941000157, -8.384220026111998791, 5.081857170174999716 ) ) ;
#7080 = CARTESIAN_POINT ( 'NONE',  ( 1.951256826536600819, 29.86029468836431278, -0.9263714941426136606 ) ) ;
#7081 = ORIENTED_EDGE ( 'NONE', *, *, #8381, .T. ) ;
#7082 = CARTESIAN_POINT ( 'NONE',  ( 23.41885967450824069, -2.987232380683592758, 8.797512113848760862 ) ) ;
#7083 = CARTESIAN_POINT ( 'NONE',  ( 20.29924913173047329, 10.29758103606868858, -2.152088117745763363 ) ) ;
#7084 = CARTESIAN_POINT ( 'NONE',  ( -0.9283276469500318928, 23.62785179069575037, -1.914674717947229654 ) ) ;
#7085 = VERTEX_POINT ( 'NONE', #22811 ) ;
#7086 = CARTESIAN_POINT ( 'NONE',  ( 24.32802197706127245, -9.050607035110887821, -9.323888775846091548 ) ) ;
#7087 = CARTESIAN_POINT ( 'NONE',  ( 4.934031413263280541, 14.29560215800634992, -3.841103650033387495 ) ) ;
#7088 =( GEOMETRIC_REPRESENTATION_CONTEXT ( 3 ) GLOBAL_UNCERTAINTY_ASSIGNED_CONTEXT ( ( #18171 ) ) GLOBAL_UNIT_ASSIGNED_CONTEXT ( ( #5688, #2171, #20583 ) ) REPRESENTATION_CONTEXT ( 'NONE', 'WORKASPACE' ) );
#7089 = CARTESIAN_POINT ( 'NONE',  ( 4.202976386093998151, 12.26255958046999694, -2.314965097242001502 ) ) ;
#7090 = VERTEX_POINT ( 'NONE', #7811 ) ;
#7091 = CARTESIAN_POINT ( 'NONE',  ( 15.88950125731000007, 9.094565878156000593, 1.328064802524999921 ) ) ;
#7092 = ORIENTED_EDGE ( 'NONE', *, *, #6254, .T. ) ;
#7093 = CARTESIAN_POINT ( 'NONE',  ( -0.8814048238219360787, 26.68195725178709310, -2.014038470394164726 ) ) ;
#7094 = CARTESIAN_POINT ( 'NONE',  ( -2.184465970885641539, 29.66666666666666075, 1.259047450927253120 ) ) ;
#7095 = ORIENTED_EDGE ( 'NONE', *, *, #13069, .F. ) ;
#7096 = CARTESIAN_POINT ( 'NONE',  ( -15.08134587121334391, -8.822584081656442478, 2.370873255088651099 ) ) ;
#7097 = CARTESIAN_POINT ( 'NONE',  ( -22.56166525371000375, 8.878912038559001019, -5.909991768459000205 ) ) ;
#7098 = EDGE_CURVE ( 'NONE', #6250, #3183, #19187, .T. ) ;
#7099 = CARTESIAN_POINT ( 'NONE',  ( -19.01137992565000445, 5.242525404089000141, 8.316352798856000206 ) ) ;
#7100 = CARTESIAN_POINT ( 'NONE',  ( 18.82829166666665799, 1.198188119826057330, -9.154452785816511451 ) ) ;
#7101 = CARTESIAN_POINT ( 'NONE',  ( -23.28944460057455501, -8.084059691274644521, 6.822389599746202293 ) ) ;
#7102 = CARTESIAN_POINT ( 'NONE',  ( -0.5748490789388736033, 27.63845388675433767, -2.129056650025603403 ) ) ;
#7103 = FACE_OUTER_BOUND ( 'NONE', #1355, .T. ) ;
#7104 = CARTESIAN_POINT ( 'NONE',  ( 1.990833611345558474, 30.65463416023253984, -0.8378372468001260565 ) ) ;
#7105 = ORIENTED_EDGE ( 'NONE', *, *, #808, .F. ) ;
#7106 = CARTESIAN_POINT ( 'NONE',  ( -2.399999999999999911, 24.50000000000000000, 0.000000000000000000 ) ) ;
#7107 = DIRECTION ( 'NONE',  ( 1.000000000000000000, 0.000000000000000000, 0.000000000000000000 ) ) ;
#7108 = CARTESIAN_POINT ( 'NONE',  ( 1.657421040685276070, 24.74463929172237542, 1.377955417119847370 ) ) ;
#7109 = TOROIDAL_SURFACE ( 'NONE', #10210, 10.50000000000000000, 0.1000000000000000056 ) ;
#7110 = CARTESIAN_POINT ( 'NONE',  ( 0.4912911496346000217, 28.16114211382000221, -2.239169049547999890 ) ) ;
#7111 = B_SPLINE_CURVE_WITH_KNOTS ( 'NONE', 3,
 ( #4959, #21668, #10405, #10529, #6186, #14029, #21420, #3260, #5080, #19609, #17205, #17798, #14151, #2551, #12345, #10645, #8585, #12461, #3018, #604, #1193, #18032, #19735, #15948, #8834, #21545, #9941, #12219, #23340, #14388, #16196, #17913, #7000, #21781, #5194, #19021, #2432, #6757, #9822, #22889, #15380, #8005, #22769, #20966, #1316, #8705, #4376, #16069, #19139, #23468, #6878, #17327, #731, #14272, #15502, #6305, #4836, #10990, #10765, #16782, #14844, #20432, #188, #22014, #1561, #21895, #18493, #18375, #11110, #18616, #16428, #9296, #20199, #7581, #14502, #76, #14960, #1666, #3606, #5649, #5427, #22356, #9410, #22234, #16669, #23941, #9173, #1906, #3383, #13035, #18159, #12810, #12576, #9056, #1785, #16550, #8946, #16313, #23704, #3843, #14732, #7112 ),
 .UNSPECIFIED., .F., .F.,
 ( 4, 1, 1, 1, 1, 1, 2, 2, 2, 1, 1, 1, 1, 2, 2, 2, 1, 1, 1, 2, 2, 2, 1, 1, 1, 1, 2, 2, 2, 2, 1, 1, 1, 2, 2, 2, 2, 2, 1, 1, 1, 2, 2, 2, 2, 1, 1, 1, 2, 2, 2, 1, 1, 1, 2, 2, 2, 1, 1, 1, 2, 2, 2, 1, 2, 2, 4 ),
 ( 0.000000000000000000, 0.06249999999999630851, 0.09374999999999449052, 0.1093749999999935330, 0.1171874999999930889, 0.1210937499999928946, 0.1230468749999928113, 0.1249999999999927558, 0.1874999999999895361, 0.2187499999999878708, 0.2343749999999870381, 0.2421874999999866218, 0.2460937499999863998, 0.2480468749999863165, 0.2499999999999862332, 0.2812499999999854561, 0.2968749999999850675, 0.3046874999999850120, 0.3085937499999849565, 0.3105468749999849010, 0.3124999999999847899, 0.3437499999999842903, 0.3593749999999841238, 0.3671874999999840128, 0.3710937499999839573, 0.3730468749999839018, 0.3740234374999838463, 0.3749999999999837907, 0.4062499999999852895, 0.4218749999999860112, 0.4296874999999864553, 0.4335937499999866773, 0.4355468749999868439, 0.4365234374999868994, 0.4374999999999868994, 0.4999999999999902300, 0.5312499999999917843, 0.5468749999999926725, 0.5546874999999931166, 0.5585937499999933387, 0.5605468749999934497, 0.5615234374999934497, 0.5624999999999935607, 0.5937499999999940048, 0.6093749999999942268, 0.6171874999999943379, 0.6210937499999943379, 0.6230468749999943379, 0.6240234374999942268, 0.6249999999999941158, 0.6562499999999938938, 0.6718749999999937828, 0.6796874999999935607, 0.6835937499999934497, 0.6855468749999934497, 0.6874999999999934497, 0.7187499999999924505, 0.7343749999999917843, 0.7421874999999915623, 0.7460937499999914513, 0.7480468749999914513, 0.7499999999999914513, 0.8124999999999935607, 0.8437499999999946709, 0.8593749999999952260, 0.8749999999999956701, 1.000000000000000000 ),
 .UNSPECIFIED. ) ;
#7112 = CARTESIAN_POINT ( 'NONE',  ( 4.835083642289389694, 12.44448910615697912, 0.3758261001295359338 ) ) ;
#7113 = ORIENTED_EDGE ( 'NONE', *, *, #5708, .F. ) ;
#7114 = CARTESIAN_POINT ( 'NONE',  ( -1.916536428469591602, 11.63903121779952166, -4.419911752329476862 ) ) ;
#7115 = CARTESIAN_POINT ( 'NONE',  ( -10.60253945176744850, 15.46640669614848029, 1.465117989003546839 ) ) ;
#7116 = CARTESIAN_POINT ( 'NONE',  ( 1.327700301679965333, 30.30949148887719957, 1.851068045074677926 ) ) ;
#7117 = AXIS2_PLACEMENT_3D ( 'NONE', #10447, #5342, #12386 ) ;
#7118 = ORIENTED_EDGE ( 'NONE', *, *, #20674, .T. ) ;
#7119 = CARTESIAN_POINT ( 'NONE',  ( 0.3272492347489778242, 24.21666666666666856, 2.499999999999994671 ) ) ;
#7120 = DIRECTION ( 'NONE',  ( -0.000000000000000000, 1.000000000000000000, -0.000000000000000000 ) ) ;
#7121 = CARTESIAN_POINT ( 'NONE',  ( 16.57406392130999961, -0.9113449805282999305, 9.675305505412000073 ) ) ;
#7122 = CARTESIAN_POINT ( 'NONE',  ( 18.70295191285947212, 8.885977204415825170, 5.457387397214819025 ) ) ;
#7123 = ADVANCED_FACE ( 'NONE', ( #9988 ), #18775, .F. ) ;
#7124 = CARTESIAN_POINT ( 'NONE',  ( 0.000000000000000000, 15.44510233504000141, 0.000000000000000000 ) ) ;
#7125 = CARTESIAN_POINT ( 'NONE',  ( -0.3060659231994000140, 30.06582184614000042, -2.321695786394999850 ) ) ;
#7126 = AXIS2_PLACEMENT_3D ( 'NONE', #12675, #3696, #11086 ) ;
#7127 = CARTESIAN_POINT ( 'NONE',  ( 17.90046080085999947, -5.121794679728999711, -10.20598855136000083 ) ) ;
#7128 = CARTESIAN_POINT ( 'NONE',  ( 13.50000000000000000, -9.665509359224504493, 1.178091801883024647 ) ) ;
#7129 = ORIENTED_EDGE ( 'NONE', *, *, #20589, .T. ) ;
#7130 = DIRECTION ( 'NONE',  ( 0.000000000000000000, 0.000000000000000000, 1.000000000000000000 ) ) ;
#7131 = CARTESIAN_POINT ( 'NONE',  ( 21.54099403953999925, -4.622832731814000340, -10.30527021446000013 ) ) ;
#7132 = DIRECTION ( 'NONE',  ( 0.000000000000000000, 0.000000000000000000, 1.000000000000000000 ) ) ;
#7133 = CARTESIAN_POINT ( 'NONE',  ( 13.55583115916570591, -6.549353884295403105, 8.008559588132170504 ) ) ;
#7134 = CARTESIAN_POINT ( 'NONE',  ( -3.950971430524645722, 13.90373848699781156, 4.848256008918679250 ) ) ;
#7135 = AXIS2_PLACEMENT_3D ( 'NONE', #4865, #1590, #4989 ) ;
#7136 = CARTESIAN_POINT ( 'NONE',  ( -12.25000000000000000, 13.93375672974001311, 0.000000000000000000 ) ) ;
#7137 = EDGE_CURVE ( 'NONE', #8984, #23190, #1210, .T. ) ;
#7138 = CARTESIAN_POINT ( 'NONE',  ( 12.50000000000000000, 13.93375672974000068, -0.1443254485109999874 ) ) ;
#7139 = ORIENTED_EDGE ( 'NONE', *, *, #2363, .F. ) ;
#7140 = CARTESIAN_POINT ( 'NONE',  ( -14.70932910584000020, -9.048752088456000209, 0.000000000000000000 ) ) ;
#7141 = CARTESIAN_POINT ( 'NONE',  ( -4.000000000000000000, 26.20000000000000284, 2.309401076759000304 ) ) ;
#7142 = ORIENTED_EDGE ( 'NONE', *, *, #12622, .T. ) ;
#7143 = DIRECTION ( 'NONE',  ( 0.000000000000000000, 0.000000000000000000, -1.000000000000000000 ) ) ;
#7144 = FACE_OUTER_BOUND ( 'NONE', #8446, .T. ) ;
#7145 = CARTESIAN_POINT ( 'NONE',  ( -2.184465970885646424, 27.93333333333333712, -1.259047450927245126 ) ) ;
#7146 = EDGE_CURVE ( 'NONE', #12189, #13776, #23722, .T. ) ;
#7147 = VERTEX_POINT ( 'NONE', #12535 ) ;
#7148 = CARTESIAN_POINT ( 'NONE',  ( 0.6124999999999999334, 1.217145837503000065E-14, 0.000000000000000000 ) ) ;
#7149 = AXIS2_PLACEMENT_3D ( 'NONE', #18423, #7509, #5818 ) ;
#7150 = DIRECTION ( 'NONE',  ( 0.000000000000000000, 1.000000000000000000, 0.000000000000000000 ) ) ;
#7151 = CARTESIAN_POINT ( 'NONE',  ( -4.000000000000117240, 24.49999999999976907, 0.3805779584833384743 ) ) ;
#7152 = ADVANCED_FACE ( 'NONE', ( #16021 ), #6597, .F. ) ;
#7153 = EDGE_LOOP ( 'NONE', ( #21700, #17851, #19296, #16433 ) ) ;
#7154 = CARTESIAN_POINT ( 'NONE',  ( -10.30434581488849766, 15.71366939120218831, -1.198334145822568253 ) ) ;
#7155 = CARTESIAN_POINT ( 'NONE',  ( -2.049853467200000168, 23.68059248353999990, -0.1598001849699000054 ) ) ;
#7156 = CARTESIAN_POINT ( 'NONE',  ( 14.42245774912164258, -1.407376103902506781, -10.22147709090256740 ) ) ;
#7157 = DIRECTION ( 'NONE',  ( 0.000000000000000000, 1.000000000000000000, 0.000000000000000000 ) ) ;
#7158 = CARTESIAN_POINT ( 'NONE',  ( 20.23448115697999938, 11.04732755767000008, 1.830078991042999759 ) ) ;
#7159 = DIRECTION ( 'NONE',  ( 0.000000000000000000, 0.000000000000000000, -1.000000000000000000 ) ) ;
#7160 = CARTESIAN_POINT ( 'NONE',  ( 13.63441501275057455, 7.583512906543072418, -4.912741062689508276 ) ) ;
#7161 = CARTESIAN_POINT ( 'NONE',  ( 0.000000000000000000, 24.49999999999999645, -2.949999999999969091 ) ) ;
#7162 = DIRECTION ( 'NONE',  ( 0.000000000000000000, -1.000000000000000000, 0.000000000000000000 ) ) ;
#7163 = EDGE_CURVE ( 'NONE', #18008, #9228, #9377, .T. ) ;
#7164 = VERTEX_POINT ( 'NONE', #21497 ) ;
#7165 = DIRECTION ( 'NONE',  ( 0.000000000000000000, -1.000000000000000000, 0.000000000000000000 ) ) ;
#7166 = AXIS2_PLACEMENT_3D ( 'NONE', #10551, #17935, #7024 ) ;
#7167 = FACE_BOUND ( 'NONE', #3428, .T. ) ;
#7168 = VERTEX_POINT ( 'NONE', #12297 ) ;
#7169 = CARTESIAN_POINT ( 'NONE',  ( -6.000000000000000000, 24.99999999999999645, -6.000000000000000000 ) ) ;
#7170 = CARTESIAN_POINT ( 'NONE',  ( 11.40904387244264839, -12.29944272054649090, -3.696645716843500296 ) ) ;
#7171 = DIRECTION ( 'NONE',  ( -1.000000000000000000, 0.000000000000000000, 0.000000000000000000 ) ) ;
#7172 = CARTESIAN_POINT ( 'NONE',  ( 16.28334066915000022, 6.390059127348000523, -9.032722790995999063 ) ) ;
#7173 = CARTESIAN_POINT ( 'NONE',  ( -14.44665740082351313, 5.895018559233071720, 8.513858593212594528 ) ) ;
#7174 = EDGE_LOOP ( 'NONE', ( #3910, #16096, #1336, #19890 ) ) ;
#7175 = CARTESIAN_POINT ( 'NONE',  ( -11.63274756584999992, 10.81900388182999961, 10.19838060593999884 ) ) ;
#7176 = CARTESIAN_POINT ( 'NONE',  ( 13.50000000000000000, 3.113621395416312776, 9.816120523786178609 ) ) ;
#7177 = DIRECTION ( 'NONE',  ( 0.000000000000000000, 0.000000000000000000, 1.000000000000000000 ) ) ;
#7178 = EDGE_CURVE ( 'NONE', #8876, #9820, #17885, .T. ) ;
#7179 = AXIS2_PLACEMENT_3D ( 'NONE', #5985, #8176, #2356 ) ;
#7180 = ORIENTED_EDGE ( 'NONE', *, *, #21504, .F. ) ;
#7181 = EDGE_CURVE ( 'NONE', #14234, #16706, #8345, .T. ) ;
#7182 = B_SPLINE_CURVE_WITH_KNOTS ( 'NONE', 3,
 ( #8445, #19828, #1415, #10742, #18135 ),
 .UNSPECIFIED., .F., .F.,
 ( 4, 1, 4 ),
 ( 0.4999999972379591262, 0.6666666666667000474, 1.000000000000000000 ),
 .UNSPECIFIED. ) ;
#7183 = CARTESIAN_POINT ( 'NONE',  ( 20.76445358373760897, -5.248161719249965884, 9.136987755281875678 ) ) ;
#7184 = AXIS2_PLACEMENT_3D ( 'NONE', #19424, #10216, #17359 ) ;
#7185 = DIRECTION ( 'NONE',  ( 0.000000000000000000, 1.000000000000000000, 0.000000000000000000 ) ) ;
#7186 = CARTESIAN_POINT ( 'NONE',  ( 16.10220164495252604, -5.930837905678782107, -8.497072249795241561 ) ) ;
#7187 = CARTESIAN_POINT ( 'NONE',  ( -18.80815922653999905, -4.543843182026999550, -10.15237538699000019 ) ) ;
#7188 = CARTESIAN_POINT ( 'NONE',  ( 1.444497674103000007, 29.12979332792999898, -1.844707417364999991 ) ) ;
#7189 = CARTESIAN_POINT ( 'NONE',  ( -16.97676503447000229, -7.308902056012999360, 6.489539471208999544 ) ) ;
#7190 = CARTESIAN_POINT ( 'NONE',  ( 1.230364976846351821, 29.92667673716075427, -1.776183484651385758 ) ) ;
#7191 = EDGE_CURVE ( 'NONE', #6055, #4848, #23431, .T. ) ;
#7192 = VERTEX_POINT ( 'NONE', #6958 ) ;
#7193 = CARTESIAN_POINT ( 'NONE',  ( 23.68327827309638423, -8.806622002366150781, 2.989114013944147885 ) ) ;
#7194 = EDGE_CURVE ( 'NONE', #14748, #21798, #5729, .T. ) ;
#7195 = CARTESIAN_POINT ( 'NONE',  ( 20.52623620103448232, 8.810251038339160345, 5.766288655265187302 ) ) ;
#7196 = CARTESIAN_POINT ( 'NONE',  ( -0.8631307901486540146, 23.64762543080364310, -1.966548252814039000 ) ) ;
#7197 = EDGE_LOOP ( 'NONE', ( #21888, #814, #17084, #22887 ) ) ;
#7198 = CARTESIAN_POINT ( 'NONE',  ( -1.350411050691750381, 23.74852911982829085, 1.803795205562840787 ) ) ;
#7199 = AXIS2_PLACEMENT_3D ( 'NONE', #7652, #22421, #18672 ) ;
#7200 = AXIS2_PLACEMENT_3D ( 'NONE', #3190, #10572, #17958 ) ;
#7201 = CARTESIAN_POINT ( 'NONE',  ( 4.778349813156999915, 12.47891620327999718, 0.1052890627751000563 ) ) ;
#7202 = EDGE_LOOP ( 'NONE', ( #13058, #5479, #14168, #6291 ) ) ;
#7203 = DIRECTION ( 'NONE',  ( 0.000000000000000000, -1.000000000000000000, 0.000000000000000000 ) ) ;
#7204 = ORIENTED_EDGE ( 'NONE', *, *, #18602, .F. ) ;
#7205 = CARTESIAN_POINT ( 'NONE',  ( -4.901008216611518975, 15.80730880277564410, 3.675502705389401825 ) ) ;
#7206 = LINE ( 'NONE', #3589, #17946 ) ;
#7207 = ORIENTED_EDGE ( 'NONE', *, *, #15591, .F. ) ;
#7208 = VECTOR ( 'NONE', #3114, 1000.000000000000000 ) ;
#7209 = CARTESIAN_POINT ( 'NONE',  ( 22.40045603379666161, -8.079183748319792358, -4.656405030027713110 ) ) ;
#7210 = B_SPLINE_CURVE_WITH_KNOTS ( 'NONE', 3,
 ( #13891, #19722, #15576, #12091, #927 ),
 .UNSPECIFIED., .F., .F.,
 ( 4, 1, 4 ),
 ( 0.000000000000000000, 0.5000000000000000000, 1.000000000000000000 ),
 .UNSPECIFIED. ) ;
#7211 = CARTESIAN_POINT ( 'NONE',  ( -20.63462503408999993, 10.41122961072999864, -2.064309927181999793 ) ) ;
#7212 = CARTESIAN_POINT ( 'NONE',  ( -20.36558224544999973, -7.982288314729000689, 4.838215421970999408 ) ) ;
#7213 = CARTESIAN_POINT ( 'NONE',  ( -4.783137886507999426, 13.34123574856998218, -4.957011659754998689 ) ) ;
#7214 = CARTESIAN_POINT ( 'NONE',  ( -22.90341771435761942, -8.498744592154324096, -6.277662391787633744 ) ) ;
#7215 = CARTESIAN_POINT ( 'NONE',  ( -7.034000000000000696, 1.310788454998999989E-14, 0.000000000000000000 ) ) ;
#7216 = CIRCLE ( 'NONE', #638, 0.5500000000000001554 ) ;
#7217 = CARTESIAN_POINT ( 'NONE',  ( -2.857252503208999705, 28.04750240010000084, -0.2814148094396999866 ) ) ;
#7218 = DIRECTION ( 'NONE',  ( 0.000000000000000000, 1.000000000000000000, 0.000000000000000000 ) ) ;
#7219 = ORIENTED_EDGE ( 'NONE', *, *, #10262, .F. ) ;
#7220 = CARTESIAN_POINT ( 'NONE',  ( 6.356497079780072168E-07, 30.81706029784504963, -2.183072574220335849 ) ) ;
#7221 = CARTESIAN_POINT ( 'NONE',  ( -10.04281598263999875, 16.40330333354999937, -1.000000000000000000 ) ) ;
#7222 = CARTESIAN_POINT ( 'NONE',  ( 4.749999920006001020, 24.30000007999099765, 4.227385663729999829E-08 ) ) ;
#7223 = CARTESIAN_POINT ( 'NONE',  ( -2.283846754818999791, 27.04021896306000272, 0.1346854910758999990 ) ) ;
#7224 = CIRCLE ( 'NONE', #20765, 0.9999999984430005817 ) ;
#7225 = CARTESIAN_POINT ( 'NONE',  ( -24.50000000000000000, 10.82531754731000007, 6.250000000000000000 ) ) ;
#7226 = ORIENTED_EDGE ( 'NONE', *, *, #190, .F. ) ;
#7227 = CIRCLE ( 'NONE', #5308, 13.75000000000000000 ) ;
#7228 = CARTESIAN_POINT ( 'NONE',  ( -0.8487876267396665675, 11.51352355685487794, -4.737227332089804399 ) ) ;
#7229 = FACE_OUTER_BOUND ( 'NONE', #7331, .T. ) ;
#7230 = VECTOR ( 'NONE', #2953, 1000.000000000000000 ) ;
#7231 = DIRECTION ( 'NONE',  ( 0.000000000000000000, 1.000000000000000000, 0.000000000000000000 ) ) ;
#7232 = ORIENTED_EDGE ( 'NONE', *, *, #17985, .F. ) ;
#7233 = DIRECTION ( 'NONE',  ( 0.000000000000000000, 1.000000000000000000, 0.000000000000000000 ) ) ;
#7234 = B_SPLINE_CURVE_WITH_KNOTS ( 'NONE', 3,
 ( #20720, #2312, #2843, #13603, #15417, #17743, #11803, #19181 ),
 .UNSPECIFIED., .F., .F.,
 ( 4, 2, 2, 4 ),
 ( 0.000000000000000000, 0.2499999999999999445, 0.4999999999999998890, 1.000000000000000000 ),
 .UNSPECIFIED. ) ;
#7235 = CARTESIAN_POINT ( 'NONE',  ( -16.32847087121332663, 1.190044756772780543, -9.090302457316877138 ) ) ;
#7236 = CARTESIAN_POINT ( 'NONE',  ( 18.35550158530999809, 7.854726640733000309, 6.622681824707000509 ) ) ;
#7237 = CARTESIAN_POINT ( 'NONE',  ( 18.68520931625605641, 9.205899787919600286, 4.917199649007022444 ) ) ;
#7238 = UNCERTAINTY_MEASURE_WITH_UNIT (LENGTH_MEASURE( 1.000000000000000082E-05 ), #12292, 'distance_accuracy_value', 'NONE');
#7239 = DIRECTION ( 'NONE',  ( 0.000000000000000000, 1.000000000000000000, 0.000000000000000000 ) ) ;
#7240 = CARTESIAN_POINT ( 'NONE',  ( -0.3083377756936999670, 28.72503243337000001, 2.063798408617000035 ) ) ;
#7241 = CARTESIAN_POINT ( 'NONE',  ( -14.25243324638999809, -7.716878364870000340, 11.63397459621999985 ) ) ;
#7242 = CARTESIAN_POINT ( 'NONE',  ( 13.50000000000000000, -4.865356088987999428, 9.073685197596999430 ) ) ;
#7243 = AXIS2_PLACEMENT_3D ( 'NONE', #701, #8111, #6522 ) ;
#7244 = VERTEX_POINT ( 'NONE', #16386 ) ;
#7245 = DIRECTION ( 'NONE',  ( -1.000000000000000000, 0.000000000000000000, 0.000000000000000000 ) ) ;
#7246 = CARTESIAN_POINT ( 'NONE',  ( 20.47869942662000042, 9.225975305757000200, 6.464965578640000210 ) ) ;
#7247 = CARTESIAN_POINT ( 'NONE',  ( -3.099999776787000005, 20.00000022320933013, -5.570936493763999179E-07 ) ) ;
#7248 = CONICAL_SURFACE ( 'NONE', #7632, 13.23032192316000000, 1.093540295016705466 ) ;
#7249 = DIRECTION ( 'NONE',  ( 0.000000000000000000, 0.000000000000000000, -1.000000000000000000 ) ) ;
#7250 = CARTESIAN_POINT ( 'NONE',  ( -4.080056528100000079, 28.00000000000000000, 4.563746053395999702 ) ) ;
#7251 = CARTESIAN_POINT ( 'NONE',  ( -9.042815982636001948, 21.50000000000000000, 1.000000000000000000 ) ) ;
#7252 = CARTESIAN_POINT ( 'NONE',  ( -0.8751670430457477723, 29.25681791730888293, -1.975049169652319581 ) ) ;
#7253 = CARTESIAN_POINT ( 'NONE',  ( -12.25000000000000000, 12.83205029844341460, -7.862349573137913161 ) ) ;
#7254 = ORIENTED_EDGE ( 'NONE', *, *, #10548, .T. ) ;
#7255 = DIRECTION ( 'NONE',  ( 0.000000000000000000, 0.000000000000000000, 1.000000000000000000 ) ) ;
#7256 = ORIENTED_EDGE ( 'NONE', *, *, #14594, .T. ) ;
#7257 = EDGE_CURVE ( 'NONE', #18186, #18240, #23778, .T. ) ;
#7258 = CARTESIAN_POINT ( 'NONE',  ( 6.274337143909004766, 13.70212203095000447, 0.1150566321023998723 ) ) ;
#7259 = LINE ( 'NONE', #11024, #21951 ) ;
#7260 = CIRCLE ( 'NONE', #21186, 3.850000000000000977 ) ;
#7261 = CYLINDRICAL_SURFACE ( 'NONE', #18078, 12.44999999999999929 ) ;
#7262 = CARTESIAN_POINT ( 'NONE',  ( 24.50000000000000000, 0.000000000000000000, 0.000000000000000000 ) ) ;
#7263 = CARTESIAN_POINT ( 'NONE',  ( 18.49162674931000083, 10.23722398798000022, 3.399059637929999766 ) ) ;
#7264 = ORIENTED_EDGE ( 'NONE', *, *, #12758, .T. ) ;
#7265 = FACE_OUTER_BOUND ( 'NONE', #1786, .T. ) ;
#7266 = CARTESIAN_POINT ( 'NONE',  ( 2.948682383037186217, 22.00131761696259503, 0.000000000000000000 ) ) ;
#7267 = VECTOR ( 'NONE', #15880, 1000.000000000000000 ) ;
#7268 = CARTESIAN_POINT ( 'NONE',  ( 23.99999963380687618, 13.93375672974000246, -1.355252715606880543E-17 ) ) ;
#7269 = ORIENTED_EDGE ( 'NONE', *, *, #7285, .T. ) ;
#7270 = ADVANCED_FACE ( 'NONE', ( #7667 ), #16627, .F. ) ;
#7271 = FACE_OUTER_BOUND ( 'NONE', #2934, .T. ) ;
#7272 = CARTESIAN_POINT ( 'NONE',  ( -0.2813946553678000062, 25.47374368677000334, 2.126068569715000134 ) ) ;
#7273 = CARTESIAN_POINT ( 'NONE',  ( 14.88762324588007679, 10.27475985081747467, -1.077678046861461736 ) ) ;
#7274 = DIRECTION ( 'NONE',  ( 0.000000000000000000, 1.000000000000000000, 0.000000000000000000 ) ) ;
#7275 = CARTESIAN_POINT ( 'NONE',  ( 18.91272705013000177, 2.168976607551000413, 10.20678623380999994 ) ) ;
#7276 = CARTESIAN_POINT ( 'NONE',  ( -1.050320413202000092, 30.22610362754999969, 1.896578797062999922 ) ) ;
#7277 = CARTESIAN_POINT ( 'NONE',  ( 13.69815667207068977, 8.472763392864036902, -3.097978430159455954 ) ) ;
#7278 = CARTESIAN_POINT ( 'NONE',  ( 4.812800256644999664, 12.64283093136000424, 0.1074564704997999637 ) ) ;
#7279 = AXIS2_PLACEMENT_3D ( 'NONE', #22419, #20602, #20846 ) ;
#7280 = VERTEX_POINT ( 'NONE', #18452 ) ;
#7281 = CARTESIAN_POINT ( 'NONE',  ( -14.73482540465084689, -5.357977798521391222, -7.317081367224309574 ) ) ;
#7282 = B_SPLINE_CURVE_WITH_KNOTS ( 'NONE', 3,
 ( #4872, #15867, #1596, #10446, #1228 ),
 .UNSPECIFIED., .F., .F.,
 ( 4, 1, 4 ),
 ( 0.000000000000000000, 0.5000000000000000000, 1.000000000000000000 ),
 .UNSPECIFIED. ) ;
#7283 = CARTESIAN_POINT ( 'NONE',  ( -2.000000000000000000, 26.50000000000000355, -3.464101615137999968 ) ) ;
#7284 = ORIENTED_EDGE ( 'NONE', *, *, #18849, .T. ) ;
#7285 = EDGE_CURVE ( 'NONE', #15508, #1857, #22313, .T. ) ;
#7286 = CARTESIAN_POINT ( 'NONE',  ( -2.388006305967797732E-16, 9.050044887908999414, 1.949955127985000258 ) ) ;
#7287 = CARTESIAN_POINT ( 'NONE',  ( 0.000000000000000000, 24.49999999999999645, 0.000000000000000000 ) ) ;
#7288 = CARTESIAN_POINT ( 'NONE',  ( 0.000000000000000000, 20.10000000000000142, 0.000000000000000000 ) ) ;
#7289 = AXIS2_PLACEMENT_3D ( 'NONE', #67, #10755, #22227 ) ;
#7290 = AXIS2_PLACEMENT_3D ( 'NONE', #18040, #1446, #8842 ) ;
#7291 = CARTESIAN_POINT ( 'NONE',  ( 14.29838079285000063, 0.2591618801014000106, -11.00707472443999890 ) ) ;
#7292 = CARTESIAN_POINT ( 'NONE',  ( -14.02798884238528565, -7.733277215070094357, 6.870939237852974557 ) ) ;
#7293 = CARTESIAN_POINT ( 'NONE',  ( 0.5899383557787000187, 28.40169433610000027, 2.621867217767999581 ) ) ;
#7294 = VERTEX_POINT ( 'NONE', #13116 ) ;
#7295 = CARTESIAN_POINT ( 'NONE',  ( -9.181633638770000161, 11.42978193837999967, -10.04780447355000028 ) ) ;
#7296 = AXIS2_PLACEMENT_3D ( 'NONE', #23096, #4342, #13655 ) ;
#7297 = CARTESIAN_POINT ( 'NONE',  ( 13.50000000000000000, 5.257133879617095218, 8.639483096027150921 ) ) ;
#7298 = CARTESIAN_POINT ( 'NONE',  ( -14.32799102833200244, -13.40593186267523329, -1.779780195184996749 ) ) ;
#7299 = EDGE_LOOP ( 'NONE', ( #12500, #10968, #8388, #7765, #13753 ) ) ;
#7300 = ADVANCED_FACE ( 'NONE', ( #20514, #14574 ), #3919, .F. ) ;
#7301 = CARTESIAN_POINT ( 'NONE',  ( 23.67649762116742096, 9.825750814993579496, -4.009899241536614589 ) ) ;
#7302 = CARTESIAN_POINT ( 'NONE',  ( 24.50000000000000711, 10.56912816078165562, -6.693733033818888956 ) ) ;
#7303 = CARTESIAN_POINT ( 'NONE',  ( 16.10209092903769701, -5.933957400870331078, -8.494887192401384013 ) ) ;
#7304 = B_SPLINE_CURVE_WITH_KNOTS ( 'NONE', 3,
 ( #5773, #17234, #18373, #187, #7579, #1784, #15531, #75, #23940, #7460, #14842, #19175, #15411, #764, #14958, #3961, #22127, #22355, #17361, #7347, #22918, #19052, #2463 ),
 .UNSPECIFIED., .F., .F.,
 ( 4, 2, 2, 2, 2, 1, 2, 2, 2, 2, 2, 4 ),
 ( 0.000000000000000000, 0.2499999999999582556, 0.3749999999999373834, 0.4374999999999283906, 0.4999999999999193978, 0.5624999999999104050, 0.5937499999999095168, 0.6249999999999086286, 0.6874999999998993028, 0.7187499999999114042, 0.7499999999999235056, 1.000000000000000000 ),
 .UNSPECIFIED. ) ;
#7305 = CARTESIAN_POINT ( 'NONE',  ( -16.24483109794999791, 4.897926442300000183, 9.908171963158000750 ) ) ;
#7306 = TOROIDAL_SURFACE ( 'NONE', #13119, 2.500000000000000000, 0.5500000000000000444 ) ;
#7307 = CARTESIAN_POINT ( 'NONE',  ( -0.7572660196559000134, 30.85628182409999809, -2.217212191475999905 ) ) ;
#7308 = CIRCLE ( 'NONE', #6924, 3.000000000000000000 ) ;
#7309 = CARTESIAN_POINT ( 'NONE',  ( -18.23630520352000062, 4.669879042777999700, -9.230749285618999878 ) ) ;
#7310 = EDGE_CURVE ( 'NONE', #12379, #14207, #7419, .T. ) ;
#7311 = CARTESIAN_POINT ( 'NONE',  ( 0.8715030722649804718, 29.95105470813893334, -1.976208964316035210 ) ) ;
#7312 = ORIENTED_EDGE ( 'NONE', *, *, #22377, .T. ) ;
#7313 = CARTESIAN_POINT ( 'NONE',  ( -0.1534377328957000075, 23.64214293815999923, -2.069255304278999841 ) ) ;
#7314 = CARTESIAN_POINT ( 'NONE',  ( 21.06533049062388230, -8.103789509103517474, 6.745704132337678516 ) ) ;
#7315 = CARTESIAN_POINT ( 'NONE',  ( -0.9242717917835999719, 23.66000000000000014, -1.952260652400999996 ) ) ;
#7316 = EDGE_LOOP ( 'NONE', ( #6155, #4202, #2804 ) ) ;
#7317 = EDGE_CURVE ( 'NONE', #10530, #9818, #262, .T. ) ;
#7318 = CARTESIAN_POINT ( 'NONE',  ( -0.5949149593206247699, 24.54751201496592472, -2.281015981353338162 ) ) ;
#7319 = FACE_OUTER_BOUND ( 'NONE', #3607, .T. ) ;
#7320 = ADVANCED_FACE ( 'NONE', ( #13230 ), #9483, .F. ) ;
#7321 = CARTESIAN_POINT ( 'NONE',  ( -3.947433534395999644, 12.10275648868998211, -2.807484267057001492 ) ) ;
#7322 = ORIENTED_EDGE ( 'NONE', *, *, #6712, .F. ) ;
#7323 = AXIS2_PLACEMENT_3D ( 'NONE', #7287, #14339, #23766 ) ;
#7324 = CARTESIAN_POINT ( 'NONE',  ( 13.25700125730999979, -8.207589172378998654, -3.980341215395999832 ) ) ;
#7325 = ORIENTED_EDGE ( 'NONE', *, *, #4638, .T. ) ;
#7326 = CIRCLE ( 'NONE', #6943, 15.43375672973999357 ) ;
#7327 = CARTESIAN_POINT ( 'NONE',  ( 2.394884942776999814, 23.89488494277999919, 0.000000000000000000 ) ) ;
#7328 = AXIS2_PLACEMENT_3D ( 'NONE', #12123, #21322, #3284 ) ;
#7329 = CARTESIAN_POINT ( 'NONE',  ( -14.44600785535203791, 2.842816319751110044, -12.49998455205779102 ) ) ;
#7330 = B_SPLINE_CURVE_WITH_KNOTS ( 'NONE', 3,
 ( #17016, #18832, #19067, #13371, #9632 ),
 .UNSPECIFIED., .F., .F.,
 ( 4, 1, 4 ),
 ( 0.000000000000000000, 0.5000000000000000000, 1.000000000000000000 ),
 .UNSPECIFIED. ) ;
#7331 = EDGE_LOOP ( 'NONE', ( #2207, #4129, #14901, #7325, #12945, #1478, #8697 ) ) ;
#7332 = EDGE_CURVE ( 'NONE', #11498, #14519, #18407, .T. ) ;
#7333 = CARTESIAN_POINT ( 'NONE',  ( -22.92422353055919970, 9.261441866921273913, -1.677491911259402002 ) ) ;
#7334 = EDGE_CURVE ( 'NONE', #386, #3390, #11590, .T. ) ;
#7335 = CARTESIAN_POINT ( 'NONE',  ( -20.58263244952000193, 6.141030327595999871, 8.010145565080000196 ) ) ;
#7336 = CARTESIAN_POINT ( 'NONE',  ( 11.97297107871801458, -8.401874682647177295, -10.44762502816489480 ) ) ;
#7337 = DIRECTION ( 'NONE',  ( -1.000000000000000000, 0.000000000000000000, 0.000000000000000000 ) ) ;
#7338 = CARTESIAN_POINT ( 'NONE',  ( -23.70120661253317706, 5.594576894260432809, 8.987328952431388629 ) ) ;
#7339 = CARTESIAN_POINT ( 'NONE',  ( -0.3658598526173800214, 27.98296886073505618, 2.142157184475797393 ) ) ;
#7340 = DIRECTION ( 'NONE',  ( 1.000000000000000000, 0.000000000000000000, 0.000000000000000000 ) ) ;
#7341 = CARTESIAN_POINT ( 'NONE',  ( -0.4393762720424909118, 29.81534065533141487, 4.365128144578327429 ) ) ;
#7342 = VERTEX_POINT ( 'NONE', #3566 ) ;
#7343 = FACE_OUTER_BOUND ( 'NONE', #20526, .T. ) ;
#7344 = CARTESIAN_POINT ( 'NONE',  ( 13.74900873693342440, 3.555560787657467525, -8.351293932026473854 ) ) ;
#7345 = CARTESIAN_POINT ( 'NONE',  ( -24.28586141838234269, -1.359960862156090800, -10.51926263243713144 ) ) ;
#7346 = CARTESIAN_POINT ( 'NONE',  ( -0.6650079486839999277, 28.55114211381999922, 2.193490157264000207 ) ) ;
#7347 = CARTESIAN_POINT ( 'NONE',  ( -2.136277960958246513, 30.85236464670898471, 0.2205790306774752796 ) ) ;
#7348 = AXIS2_PLACEMENT_3D ( 'NONE', #4823, #9896, #13641 ) ;
#7349 = CARTESIAN_POINT ( 'NONE',  ( -2.000000000000000000, 18.89999999999999858, -5.041390465489999878E-11 ) ) ;
#7350 = ORIENTED_EDGE ( 'NONE', *, *, #4145, .T. ) ;
#7351 = CARTESIAN_POINT ( 'NONE',  ( 0.1315063851937676997, 11.48152553765250516, -4.814286258553329922 ) ) ;
#7352 = CARTESIAN_POINT ( 'NONE',  ( 24.50000000000000711, 11.08150693382694030, 5.806266966183555311 ) ) ;
#7353 = CARTESIAN_POINT ( 'NONE',  ( -4.000000000000000000, 28.00000000000000000, 0.000000000000000000 ) ) ;
#7354 = ORIENTED_EDGE ( 'NONE', *, *, #9343, .F. ) ;
#7355 = EDGE_CURVE ( 'NONE', #10857, #3930, #16217, .T. ) ;
#7356 = CARTESIAN_POINT ( 'NONE',  ( -1.235289751754999887, 30.50000000000000000, -2.173490103315000255 ) ) ;
#7357 = CARTESIAN_POINT ( 'NONE',  ( 18.68456408531000079, -2.737678269967000144, 9.911560247287001246 ) ) ;
#7358 = CARTESIAN_POINT ( 'NONE',  ( 18.70488052352785147, 8.850818011485689141, 5.514450890227789337 ) ) ;
#7359 = CARTESIAN_POINT ( 'NONE',  ( -2.434931691670788378, 29.06753006952332896, 0.6543697108982053923 ) ) ;
#7360 = CARTESIAN_POINT ( 'NONE',  ( 2.318031435825999687, 29.86728268470999836, -0.3326829368231999928 ) ) ;
#7361 = DIRECTION ( 'NONE',  ( 0.000000000000000000, -1.000000000000000000, 0.000000000000000000 ) ) ;
#7362 = CARTESIAN_POINT ( 'NONE',  ( 13.50000000000000178, -5.180989882992017570, 8.880677523943516505 ) ) ;
#7363 = ORIENTED_EDGE ( 'NONE', *, *, #15236, .T. ) ;
#7364 = CARTESIAN_POINT ( 'NONE',  ( -1.999167105995442562, 28.88333333333333641, 1.536366799937298300 ) ) ;
#7365 = CARTESIAN_POINT ( 'NONE',  ( 22.69754412252000009, 5.148292089747000588, 9.490647990332998774 ) ) ;
#7366 = CARTESIAN_POINT ( 'NONE',  ( 2.500000000000001776, 29.18333333333333357, 0.3272492347489251441 ) ) ;
#7367 = ORIENTED_EDGE ( 'NONE', *, *, #20031, .T. ) ;
#7368 = CARTESIAN_POINT ( 'NONE',  ( 24.50000000000000355, -7.886533982023047784, 7.073078350185027396 ) ) ;
#7369 = CARTESIAN_POINT ( 'NONE',  ( 24.50000000000000000, 3.215423653429137385, 9.789911160088649922 ) ) ;
#7370 = VECTOR ( 'NONE', #11983, 1000.000000000000000 ) ;
#7371 = CARTESIAN_POINT ( 'NONE',  ( -4.776913516551996253, 12.47840662102999509, -0.1494451571019999592 ) ) ;
#7372 = CARTESIAN_POINT ( 'NONE',  ( -0.2449543915955024187, 29.21838483711510293, -2.145887526803566647 ) ) ;
#7373 = CARTESIAN_POINT ( 'NONE',  ( -21.14116503741999864, -8.837159004920000172, 6.686531827553999996 ) ) ;
#7374 = EDGE_LOOP ( 'NONE', ( #18554, #4456 ) ) ;
#7375 = B_SPLINE_CURVE_WITH_KNOTS ( 'NONE', 3,
 ( #21444, #13927, #6657, #14172, #6903, #23243 ),
 .UNSPECIFIED., .F., .F.,
 ( 4, 2, 4 ),
 ( 0.000000000000000000, 0.5000000000000000000, 1.000000000000000000 ),
 .UNSPECIFIED. ) ;
#7376 = CARTESIAN_POINT ( 'NONE',  ( -6.125000000000000000, 21.50000000000000000, 0.000000000000000000 ) ) ;
#7377 = EDGE_LOOP ( 'NONE', ( #11864, #14543, #1249 ) ) ;
#7378 = CARTESIAN_POINT ( 'NONE',  ( -0.2920304106900999952, 25.26497464138999760, -2.335031432767999959 ) ) ;
#7379 = CARTESIAN_POINT ( 'NONE',  ( -0.3272492347489287523, 28.18333333333333357, 2.500000000000001332 ) ) ;
#7380 = CARTESIAN_POINT ( 'NONE',  ( 12.28779254563088585, 5.665119685602451050, -12.50001287414461792 ) ) ;
#7381 = DIRECTION ( 'NONE',  ( -0.7071067811868960717, 0.7071067811861969643, -5.329912173642970297E-08 ) ) ;
#7382 = CARTESIAN_POINT ( 'NONE',  ( 1.750000000000000000, 12.37689379448999993, 0.000000000000000000 ) ) ;
#7383 = CARTESIAN_POINT ( 'NONE',  ( 16.60050158530999909, 6.318772076511000257, 8.042630855556000213 ) ) ;
#7384 =( NAMED_UNIT ( * ) PLANE_ANGLE_UNIT ( ) SI_UNIT ( $, .RADIAN. ) );
#7385 = EDGE_LOOP ( 'NONE', ( #8383, #288, #20504, #524 ) ) ;
#7386 = DIRECTION ( 'NONE',  ( -1.000000000000000000, 0.000000000000000000, 0.000000000000000000 ) ) ;
#7387 = DIRECTION ( 'NONE',  ( 0.000000000000000000, 0.000000000000000000, 1.000000000000000000 ) ) ;
#7388 = DIRECTION ( 'NONE',  ( 1.000000000000000000, 0.000000000000000000, 0.000000000000000000 ) ) ;
#7389 = VERTEX_POINT ( 'NONE', #5610 ) ;
#7390 = CARTESIAN_POINT ( 'NONE',  ( -10.83200247828752971, 15.36487885975186352, -1.677940321992645645 ) ) ;
#7391 = CARTESIAN_POINT ( 'NONE',  ( 1.982157587870999826, 24.85598014098999897, -1.234381845068999839 ) ) ;
#7392 = CARTESIAN_POINT ( 'NONE',  ( 14.41647009244453947, -1.614193569338650880, -10.19093708827842271 ) ) ;
#7393 = LINE ( 'NONE', #9457, #11809 ) ;
#7394 = CARTESIAN_POINT ( 'NONE',  ( 19.27982097606999901, -9.756977011084000395, 5.441823009411000278 ) ) ;
#7395 = EDGE_CURVE ( 'NONE', #2511, #3147, #7544, .T. ) ;
#7396 = CARTESIAN_POINT ( 'NONE',  ( 0.4321025471916000171, 29.76162456898000030, -2.320663853759999729 ) ) ;
#7397 = CARTESIAN_POINT ( 'NONE',  ( 14.10157458702998667, 4.520082339245768743, 7.819331374180982230 ) ) ;
#7398 = CARTESIAN_POINT ( 'NONE',  ( -6.605774574140806266, 15.40025296468788341, -1.587926255657816643 ) ) ;
#7399 = CARTESIAN_POINT ( 'NONE',  ( -11.00000000000000000, 1.359357947053999856E-14, 0.000000000000000000 ) ) ;
#7400 = CARTESIAN_POINT ( 'NONE',  ( 12.04708237233490387, 13.35071834206844876, -1.875975938906002005 ) ) ;
#7401 = ORIENTED_EDGE ( 'NONE', *, *, #3763, .T. ) ;
#7402 = CARTESIAN_POINT ( 'NONE',  ( -4.750000000000000000, 15.09999999999999964, 0.000000000000000000 ) ) ;
#7403 = CARTESIAN_POINT ( 'NONE',  ( -14.00000000000000000, -10.27687089286999900, -0.6428416445564000270 ) ) ;
#7404 = ORIENTED_EDGE ( 'NONE', *, *, #6268, .F. ) ;
#7405 = FACE_OUTER_BOUND ( 'NONE', #17091, .T. ) ;
#7406 = FACE_OUTER_BOUND ( 'NONE', #1003, .T. ) ;
#7407 = ADVANCED_FACE ( 'NONE', ( #4149 ), #7959, .T. ) ;
#7408 = CARTESIAN_POINT ( 'NONE',  ( 21.83358103379666204, -1.208283319978287418, 9.231574434091362136 ) ) ;
#7409 = CARTESIAN_POINT ( 'NONE',  ( 18.20064194352000086, -0.4690725264157000751, -11.10709960042999889 ) ) ;
#7410 = DIRECTION ( 'NONE',  ( 0.000000000000000000, 0.000000000000000000, 1.000000000000000000 ) ) ;
#7411 = CARTESIAN_POINT ( 'NONE',  ( -2.583184600869000036, 28.24712896667000095, -0.6741018852137000694 ) ) ;
#7412 = VERTEX_POINT ( 'NONE', #18925 ) ;
#7413 = CARTESIAN_POINT ( 'NONE',  ( -10.71634506584999968, -1.748784590530000127, -14.76480909560000043 ) ) ;
#7414 = DIRECTION ( 'NONE',  ( -0.8284926070883130711, -0.5600000000000090461, 0.000000000000000000 ) ) ;
#7415 = CARTESIAN_POINT ( 'NONE',  ( -14.50000018026810089, -10.69550487835728347, -6.474840093751000225 ) ) ;
#7416 = ORIENTED_EDGE ( 'NONE', *, *, #21412, .T. ) ;
#7417 = CARTESIAN_POINT ( 'NONE',  ( -14.47793701804645217, 11.73188619686574263, 4.679765522763038810 ) ) ;
#7418 = CARTESIAN_POINT ( 'NONE',  ( 20.29382020395017250, 9.419176356032403774, 4.682166151186863523 ) ) ;
#7419 = LINE ( 'NONE', #9132, #11443 ) ;
#7420 = CARTESIAN_POINT ( 'NONE',  ( 15.94258035992931966, -9.513174729914155137, -4.100360902401353869 ) ) ;
#7421 = CARTESIAN_POINT ( 'NONE',  ( -16.60615772801000034, 10.95457934470999994, -1.541957209009000129 ) ) ;
#7422 = EDGE_CURVE ( 'NONE', #3528, #5391, #20346, .T. ) ;
#7423 = CARTESIAN_POINT ( 'NONE',  ( 1.417967650155999904, 30.30418396362999900, 1.881788475004999794 ) ) ;
#7424 = CARTESIAN_POINT ( 'NONE',  ( -16.61126241975999918, -1.906005702182999917, -10.12158796435999975 ) ) ;
#7425 = CARTESIAN_POINT ( 'NONE',  ( 1.173990260879828496, 29.93071037106722798, -1.813501616305194686 ) ) ;
#7426 = ORIENTED_EDGE ( 'NONE', *, *, #14380, .F. ) ;
#7427 = CARTESIAN_POINT ( 'NONE',  ( -0.6137755221146999896, 25.35240352290000132, 2.097951008038000165 ) ) ;
#7428 = CARTESIAN_POINT ( 'NONE',  ( 20.98021033963484427, -5.789786262372857983, 8.802753455338001132 ) ) ;
#7429 = DIRECTION ( 'NONE',  ( 0.000000000000000000, 0.000000000000000000, -1.000000000000000000 ) ) ;
#7430 = ORIENTED_EDGE ( 'NONE', *, *, #15315, .T. ) ;
#7431 = CARTESIAN_POINT ( 'NONE',  ( 24.45564077607145137, -2.060124049350608555, 12.50000000000000178 ) ) ;
#7432 = CARTESIAN_POINT ( 'NONE',  ( -6.309599240701002643, 15.06635153518999104, 3.401153641079002199 ) ) ;
#7433 = EDGE_CURVE ( 'NONE', #12102, #7085, #16838, .T. ) ;
#7434 = DIRECTION ( 'NONE',  ( 1.000000000000000000, 0.000000000000000000, 0.000000000000000000 ) ) ;
#7435 = CARTESIAN_POINT ( 'NONE',  ( 13.69575125731000043, 3.560502093102000387, -8.410767149301999979 ) ) ;
#7436 = ORIENTED_EDGE ( 'NONE', *, *, #20620, .F. ) ;
#7437 = CIRCLE ( 'NONE', #21759, 3.050000000000000266 ) ;
#7438 = CARTESIAN_POINT ( 'NONE',  ( -7.834000000000000519, -10.69999999999999929, 0.000000000000000000 ) ) ;
#7439 = EDGE_CURVE ( 'NONE', #6219, #16646, #4512, .T. ) ;
#7440 = CARTESIAN_POINT ( 'NONE',  ( 0.3272492347489455167, 29.81666666666667709, 2.499999999999998668 ) ) ;
#7441 = EDGE_LOOP ( 'NONE', ( #15373, #7264, #14822, #1211, #11103, #5507 ) ) ;
#7442 = DIRECTION ( 'NONE',  ( -0.000000000000000000, -1.000000000000000000, -0.000000000000000000 ) ) ;
#7443 = CARTESIAN_POINT ( 'NONE',  ( -4.811404347808999837, 12.64229228517000969, -0.1541852644638002090 ) ) ;
#7444 = CARTESIAN_POINT ( 'NONE',  ( 11.99999999999999822, -2.116414852691937742, -9.237906777948852621 ) ) ;
#7445 = ADVANCED_FACE ( 'NONE', ( #13464 ), #12611, .T. ) ;
#7446 = CARTESIAN_POINT ( 'NONE',  ( 11.53663804754834743, -9.092401935506826405, -9.251313393160373266 ) ) ;
#7447 = DIRECTION ( 'NONE',  ( 0.000000000000000000, -1.000000000000000000, 0.000000000000000000 ) ) ;
#7448 = CARTESIAN_POINT ( 'NONE',  ( -19.89240800188232683, -0.7325527030282151797, 10.46337770069665396 ) ) ;
#7449 = CARTESIAN_POINT ( 'NONE',  ( 0.000000000000000000, 26.50000000000000355, 0.000000000000000000 ) ) ;
#7450 = CARTESIAN_POINT ( 'NONE',  ( 15.76716666666666455, 7.930444964421201171, 4.570677355979499978 ) ) ;
#7451 = CARTESIAN_POINT ( 'NONE',  ( -5.523874320477998978, 16.26076007236001431, 2.688832781278999828 ) ) ;
#7452 = DIRECTION ( 'NONE',  ( -0.9996848865506517967, 0.000000000000000000, -0.02510234256419879503 ) ) ;
#7453 = EDGE_LOOP ( 'NONE', ( #6455, #7067, #6937, #20630 ) ) ;
#7454 = CARTESIAN_POINT ( 'NONE',  ( 19.20820820724999933, 5.862953550309000228, -7.802432380257999789 ) ) ;
#7455 = CARTESIAN_POINT ( 'NONE',  ( 14.99328936713000004, -9.056039068417000237, 0.000000000000000000 ) ) ;
#7456 = CONICAL_SURFACE ( 'NONE', #3975, 4.309401076758999416, 1.119376321708719590 ) ;
#7457 = CARTESIAN_POINT ( 'NONE',  ( -22.46506791698822170, -1.100719659442045861, -10.63859953765026312 ) ) ;
#7458 = CARTESIAN_POINT ( 'NONE',  ( -2.445277951317000209, 27.02187716036000253, 0.1442055869096000031 ) ) ;
#7459 = EDGE_CURVE ( 'NONE', #13107, #15625, #9128, .T. ) ;
#7460 = CARTESIAN_POINT ( 'NONE',  ( -2.124284333938379898, 30.86714579923354407, 0.1911072213488915206 ) ) ;
#7461 = CARTESIAN_POINT ( 'NONE',  ( -11.04281598264000053, 1.359882291614000008E-14, 0.000000000000000000 ) ) ;
#7462 = EDGE_LOOP ( 'NONE', ( #16813, #3441 ) ) ;
#7463 = CARTESIAN_POINT ( 'NONE',  ( -4.671788442614717596, 12.38274754940156264, -1.292526076544993519 ) ) ;
#7464 = CARTESIAN_POINT ( 'NONE',  ( -0.9242717917835999719, 23.66000000000000014, -1.952260652400999996 ) ) ;
#7465 = CARTESIAN_POINT ( 'NONE',  ( 0.4169900196955230176, 29.80682928967814860, -2.239500026962490953 ) ) ;
#7466 = VERTEX_POINT ( 'NONE', #9958 ) ;
#7467 = CARTESIAN_POINT ( 'NONE',  ( -12.25000000000000000, 6.613190111079999767, -13.46349570337000046 ) ) ;
#7468 = AXIS2_PLACEMENT_3D ( 'NONE', #14127, #2995, #6370 ) ;
#7469 = CARTESIAN_POINT ( 'NONE',  ( 15.61331408530999987, -8.260803322383997838, -5.986632065681000370 ) ) ;
#7470 = CARTESIAN_POINT ( 'NONE',  ( 18.39251201459628859, 8.989286056864246532, -5.271706797561602542 ) ) ;
#7471 = ADVANCED_FACE ( 'NONE', ( #747 ), #15675, .T. ) ;
#7472 = CARTESIAN_POINT ( 'NONE',  ( -23.74465998031000069, 6.216878364870000340, 12.50000000000000000 ) ) ;
#7473 = CARTESIAN_POINT ( 'NONE',  ( -0.8375484967288000515, 29.60256380282000066, 2.186883670786000433 ) ) ;
#7474 = EDGE_CURVE ( 'NONE', #7294, #13433, #17638, .T. ) ;
#7475 = DIRECTION ( 'NONE',  ( -7.335406816068161220E-08, -0.9999999999995213829, -9.756601275250212230E-07 ) ) ;
#7476 = CIRCLE ( 'NONE', #21814, 6.125000000000000000 ) ;
#7477 = CARTESIAN_POINT ( 'NONE',  ( -2.104642740648948074, 30.88517755921813901, -0.2852235104369513219 ) ) ;
#7478 = ORIENTED_EDGE ( 'NONE', *, *, #11203, .F. ) ;
#7479 = CARTESIAN_POINT ( 'NONE',  ( 4.000000000000000000, 29.69999999999999929, 2.309401076759000304 ) ) ;
#7480 = CARTESIAN_POINT ( 'NONE',  ( 22.16639681605000334, 7.771014960181000575, -7.474990234536999623 ) ) ;
#7481 = CARTESIAN_POINT ( 'NONE',  ( -24.48172546360977009, 4.179826417290672502, -9.441142365384852297 ) ) ;
#7482 = EDGE_LOOP ( 'NONE', ( #5607, #12750 ) ) ;
#7483 = FACE_OUTER_BOUND ( 'NONE', #22096, .T. ) ;
#7484 = CARTESIAN_POINT ( 'NONE',  ( -8.000000000000000000, -10.50000000000000000, 0.000000000000000000 ) ) ;
#7485 = CARTESIAN_POINT ( 'NONE',  ( 4.087091007756002092, 12.14415498498998680, 2.742727926892003509 ) ) ;
#7486 = CARTESIAN_POINT ( 'NONE',  ( -1.291923323229889231, 29.28551790513946074, -1.731104546042324221 ) ) ;
#7487 = DIRECTION ( 'NONE',  ( 0.000000000000000000, 0.000000000000000000, -1.000000000000000000 ) ) ;
#7488 = ORIENTED_EDGE ( 'NONE', *, *, #17020, .T. ) ;
#7489 = EDGE_CURVE ( 'NONE', #21635, #15998, #6013, .T. ) ;
#7490 = EDGE_CURVE ( 'NONE', #8084, #4163, #13899, .T. ) ;
#7491 = CARTESIAN_POINT ( 'NONE',  ( -0.2897094055803834389, 23.75786872615814005, 2.255733293301447784 ) ) ;
#7492 = ORIENTED_EDGE ( 'NONE', *, *, #19654, .F. ) ;
#7493 = CARTESIAN_POINT ( 'NONE',  ( 0.5753128712306000425, 24.08057988946000094, 2.281812558324999962 ) ) ;
#7494 = CARTESIAN_POINT ( 'NONE',  ( 4.918133982481998956, 14.11827433645001229, 3.900434897472001339 ) ) ;
#7495 = CARTESIAN_POINT ( 'NONE',  ( 16.54274770046333742, -5.589705041635214755, 7.273700408684123708 ) ) ;
#7496 = B_SPLINE_CURVE_WITH_KNOTS ( 'NONE', 3,
 ( #4885, #4395, #12273, #8272, #19660, #13708, #4516, #2945 ),
 .UNSPECIFIED., .F., .F.,
 ( 4, 2, 2, 4 ),
 ( 0.000000000000000000, 0.2499999999999998890, 0.4999999999999997780, 1.000000000000000000 ),
 .UNSPECIFIED. ) ;
#7497 = DIRECTION ( 'NONE',  ( 1.000000000000000000, 0.000000000000000000, 0.000000000000000000 ) ) ;
#7498 = FACE_OUTER_BOUND ( 'NONE', #9216, .T. ) ;
#7499 = CARTESIAN_POINT ( 'NONE',  ( 12.02006424930999984, -10.30839584998999925, 1.075033486111000025 ) ) ;
#7500 = AXIS2_PLACEMENT_3D ( 'NONE', #8514, #10199, #23021 ) ;
#7501 = AXIS2_PLACEMENT_3D ( 'NONE', #2229, #18821, #13484 ) ;
#7502 = CARTESIAN_POINT ( 'NONE',  ( -14.94546155477000049, -9.714114572133000891, -0.2583773470232999525 ) ) ;
#7503 = DIRECTION ( 'NONE',  ( -1.000000000000000000, 0.000000000000000000, 0.000000000000000000 ) ) ;
#7504 = DIRECTION ( 'NONE',  ( 0.5000000000000169864, -0.8660254037844288266, 0.000000000000000000 ) ) ;
#7505 = VERTEX_POINT ( 'NONE', #4881 ) ;
#7506 = CARTESIAN_POINT ( 'NONE',  ( -10.75755763812815680, 15.39137541006824250, -1.608313476896800154 ) ) ;
#7507 = CARTESIAN_POINT ( 'NONE',  ( -1.578943844734999935, 24.27961011138000202, -1.720344029022000010 ) ) ;
#7508 = CARTESIAN_POINT ( 'NONE',  ( 14.57135008224444128, 3.797263269294576471, -9.601797994946904780 ) ) ;
#7509 = DIRECTION ( 'NONE',  ( -1.000000000000000000, 0.000000000000000000, 0.000000000000000000 ) ) ;
#7510 = CARTESIAN_POINT ( 'NONE',  ( 21.62900612854999949, -7.523913936368999522, -8.345185084459998848 ) ) ;
#7511 = CARTESIAN_POINT ( 'NONE',  ( -2.395497655370999901, 30.70938692720000063, 0.5757869882262999228 ) ) ;
#7512 = CARTESIAN_POINT ( 'NONE',  ( 13.80187520366866849, 9.025291185423055751, 0.006276713024069551644 ) ) ;
#7513 = CARTESIAN_POINT ( 'NONE',  ( 4.816630038177000195, 12.64431341689999932, -0.1115539088738999873 ) ) ;
#7514 = B_SPLINE_CURVE_WITH_KNOTS ( 'NONE', 3,
 ( #16613, #11173, #21, #22888 ),
 .UNSPECIFIED., .F., .F.,
 ( 4, 4 ),
 ( 0.000000000000000000, 1.000000000000000000 ),
 .UNSPECIFIED. ) ;
#7515 = CARTESIAN_POINT ( 'NONE',  ( -5.204962792833000229, 27.25000000000000000, 2.704962792832999785 ) ) ;
#7516 = CARTESIAN_POINT ( 'NONE',  ( 11.12576011241902840, 10.20205618038153084, -7.329535452988973354 ) ) ;
#7517 = ORIENTED_EDGE ( 'NONE', *, *, #21552, .T. ) ;
#7518 = CARTESIAN_POINT ( 'NONE',  ( -2.186814738145873793, 24.16665839525370885, -1.278079063527637782 ) ) ;
#7519 = CARTESIAN_POINT ( 'NONE',  ( -3.316314694148183584, 28.12756664670259354, 2.704122461039521585 ) ) ;
#7520 = ORIENTED_EDGE ( 'NONE', *, *, #18603, .F. ) ;
#7521 = FACE_OUTER_BOUND ( 'NONE', #17022, .T. ) ;
#7522 = CARTESIAN_POINT ( 'NONE',  ( 24.50000000000000000, 10.31403833462485053, 7.135561573215231768 ) ) ;
#7523 = CARTESIAN_POINT ( 'NONE',  ( 0.000000000000000000, 29.69999999999999929, -4.618802153517000519 ) ) ;
#7524 = CIRCLE ( 'NONE', #10644, 0.5500000000000001554 ) ;
#7525 = CARTESIAN_POINT ( 'NONE',  ( 14.98635508327000032, 10.44157347027999982, 3.551293096755000267 ) ) ;
#7526 = CARTESIAN_POINT ( 'NONE',  ( -6.171953915136863422, 15.86494870466900764, 1.104274664945693374 ) ) ;
#7527 = ORIENTED_CLOSED_SHELL ( 'NONE', *, #23556, .F. );
#7528 = CARTESIAN_POINT ( 'NONE',  ( -0.6741018852137999895, 25.71212896666999725, -2.583184600869000036 ) ) ;
#7529 = EDGE_LOOP ( 'NONE', ( #18559, #7901, #16211, #11593, #7854, #6173, #11289, #20673, #13904 ) ) ;
#7530 = ORIENTED_EDGE ( 'NONE', *, *, #22509, .F. ) ;
#7531 = AXIS2_PLACEMENT_3D ( 'NONE', #15766, #1246, #21352 ) ;
#7532 = CARTESIAN_POINT ( 'NONE',  ( -9.588923638769999869, -11.49744000511999964, -9.970428444189000317 ) ) ;
#7533 = DIRECTION ( 'NONE',  ( 1.000000000000000000, 0.000000000000000000, 0.000000000000000000 ) ) ;
#7534 = CARTESIAN_POINT ( 'NONE',  ( -14.25851235546000062, -6.966599976214999934, 12.06714802587000079 ) ) ;
#7535 = ORIENTED_EDGE ( 'NONE', *, *, #19989, .T. ) ;
#7536 = CARTESIAN_POINT ( 'NONE',  ( -14.29262082160887637, 13.66753291840703710, 1.327138571200180861 ) ) ;
#7537 = CARTESIAN_POINT ( 'NONE',  ( -21.96532910583999865, -9.234955349282000014, 0.000000000000000000 ) ) ;
#7538 = B_SPLINE_CURVE_WITH_KNOTS ( 'NONE', 3,
 ( #6216, #13844, #17363, #1006, #4530, #6089 ),
 .UNSPECIFIED., .F., .F.,
 ( 4, 2, 4 ),
 ( 0.000000000000000000, 0.5000000000000000000, 1.000000000000000000 ),
 .UNSPECIFIED. ) ;
#7539 = CARTESIAN_POINT ( 'NONE',  ( 24.48327518124252933, 10.18191985984368664, -7.364397484155817963 ) ) ;
#7540 = CARTESIAN_POINT ( 'NONE',  ( 15.89621519439380570, -10.03933691619746682, -2.545899918998145939 ) ) ;
#7541 = CARTESIAN_POINT ( 'NONE',  ( -18.41279087833000006, 11.03951774085000004, -1.267611736511999876 ) ) ;
#7542 = CARTESIAN_POINT ( 'NONE',  ( 1.351857446083000180, 28.90405828138999667, -1.726400466208000140 ) ) ;
#7543 = AXIS2_PLACEMENT_3D ( 'NONE', #12242, #3039, #23359 ) ;
#7544 = B_SPLINE_CURVE_WITH_KNOTS ( 'NONE', 3,
 ( #12992, #20393, #18575, #3798, #11192, #9363, #16737, #14919, #8151, #2447, #22551, #865, #19037, #18801, #8269, #22904, #5957, #6200, #7904, #16988, #17105, #20623, #389, #15273, #6320, #11427, #19157, #4277, #15633, #13342, #15516, #23024, #9723, #11665, #13705, #22784, #15156, #4033, #20741, #11545, #7786, #17221, #2567, #2210, #21098, #9601, #20867, #6441 ),
 .UNSPECIFIED., .F., .F.,
 ( 4, 2, 2, 2, 2, 2, 1, 1, 2, 2, 2, 1, 1, 1, 2, 2, 2, 2, 1, 1, 1, 2, 2, 2, 1, 1, 2, 2, 4 ),
 ( 0.000000000000000000, 0.06250000000000340006, 0.09375000000000510703, 0.1250000000000068001, 0.1875000000000106859, 0.2187500000000128786, 0.2343750000000139333, 0.2421875000000143219, 0.2460937500000142386, 0.2500000000000142109, 0.3750000000000117684, 0.4375000000000104916, 0.4687500000000101585, 0.4843750000000100475, 0.4921875000000094924, 0.5000000000000089928, 0.6249999999999866773, 0.6874999999999755751, 0.7187499999999699130, 0.7343749999999678035, 0.7421874999999668043, 0.7460937499999671374, 0.7499999999999673594, 0.8124999999999765743, 0.8437499999999816813, 0.8593749999999849010, 0.8671874999999856781, 0.8749999999999864553, 1.000000000000000000 ),
 .UNSPECIFIED. ) ;
#7545 = CARTESIAN_POINT ( 'NONE',  ( -18.07393293677000301, 10.37468091520999991, 3.263143967163999903 ) ) ;
#7546 = CARTESIAN_POINT ( 'NONE',  ( 1.303752836300308804, 29.68620654978850482, 1.722188842540592457 ) ) ;
#7547 = EDGE_LOOP ( 'NONE', ( #13442, #10504, #986, #13788 ) ) ;
#7548 = CARTESIAN_POINT ( 'NONE',  ( -1.279456652065000144, 24.74056538345000078, 1.954075669677000082 ) ) ;
#7549 = CARTESIAN_POINT ( 'NONE',  ( 21.37743771091500378, -9.903291219543641333, -4.060970818798163684 ) ) ;
#7550 = CARTESIAN_POINT ( 'NONE',  ( -22.87210175995843642, 9.258583067823760615, -6.329161777784410158E-06 ) ) ;
#7551 = ORIENTED_EDGE ( 'NONE', *, *, #11360, .F. ) ;
#7552 = CARTESIAN_POINT ( 'NONE',  ( 2.384000448764866054, 30.27849728015833719, -0.8693082857020455467 ) ) ;
#7553 = DIRECTION ( 'NONE',  ( 1.877655941804990996E-08, -0.9999999999999978906, -6.187284376306977451E-08 ) ) ;
#7554 = ADVANCED_FACE ( 'NONE', ( #8751, #8879 ), #17596, .F. ) ;
#7555 = CARTESIAN_POINT ( 'NONE',  ( 16.79343892131000260, -7.329510781495000238, 6.390029238976000059 ) ) ;
#7556 = EDGE_LOOP ( 'NONE', ( #22967, #5937, #17008, #10196 ) ) ;
#7557 = AXIS2_PLACEMENT_3D ( 'NONE', #9813, #6297, #21200 ) ;
#7558 = CARTESIAN_POINT ( 'NONE',  ( -5.264900118121860650, 16.02290957484199652, 3.131682802096217966 ) ) ;
#7559 = CARTESIAN_POINT ( 'NONE',  ( 2.184465970885649977, 29.93333333333333002, 1.259047450927240686 ) ) ;
#7560 = ORIENTED_EDGE ( 'NONE', *, *, #13086, .T. ) ;
#7561 = CARTESIAN_POINT ( 'NONE',  ( 23.11849770046333674, 9.264547928196073201, -1.212853435574229310 ) ) ;
#7562 = CARTESIAN_POINT ( 'NONE',  ( -4.814900992596998108, 12.64364337456001941, 0.1283334480982998294 ) ) ;
#7563 = CARTESIAN_POINT ( 'NONE',  ( 11.99999999999999822, 0.7437781458199891338, -9.269733647780308061 ) ) ;
#7564 = ADVANCED_FACE ( 'NONE', ( #12507 ), #3728, .T. ) ;
#7565 = DIRECTION ( 'NONE',  ( 0.7071067811867457475, 0.7071067811863459562, -6.966834331432447605E-08 ) ) ;
#7566 = CARTESIAN_POINT ( 'NONE',  ( -4.263376217415998148, 14.54355705694000456, -4.183184883477999882 ) ) ;
#7567 = CARTESIAN_POINT ( 'NONE',  ( -20.22696463660509636, 9.305942615553171038, 4.861376333746878053 ) ) ;
#7568 = CARTESIAN_POINT ( 'NONE',  ( -3.560623727957782148, 26.31534065533140421, -2.563075085697512634 ) ) ;
#7569 = DIRECTION ( 'NONE',  ( 0.000000000000000000, 0.000000000000000000, -1.000000000000000000 ) ) ;
#7570 = CARTESIAN_POINT ( 'NONE',  ( 0.6153010951426000075, 28.63250240009999814, -2.804372049896000085 ) ) ;
#7571 = CARTESIAN_POINT ( 'NONE',  ( -0.6752522526669163527, 30.36340219175618671, 2.051621071677199648 ) ) ;
#7572 = EDGE_LOOP ( 'NONE', ( #23487, #16760, #2724, #22101 ) ) ;
#7573 = CARTESIAN_POINT ( 'NONE',  ( 18.11311958374000142, 0.09792845715294999642, 9.251054258097999750 ) ) ;
#7574 = CARTESIAN_POINT ( 'NONE',  ( 1.659709954204918292, 24.76332575048712314, 1.345642078841861711 ) ) ;
#7575 = CONICAL_SURFACE ( 'NONE', #4492, 9.152445778720998959, 0.02565634000431304615 ) ;
#7576 = B_SPLINE_CURVE_WITH_KNOTS ( 'NONE', 3,
 ( #8369, #21204, #15861, #4619, #12010, #15738, #6549, #13933 ),
 .UNSPECIFIED., .F., .F.,
 ( 4, 2, 2, 4 ),
 ( 0.000000000000000000, 0.2500000000000000555, 0.5000000000000003331, 1.000000000000000000 ),
 .UNSPECIFIED. ) ;
#7577 = CARTESIAN_POINT ( 'NONE',  ( -23.50934654278774971, 5.808796177084403212, 8.845529366387745895 ) ) ;
#7578 = CARTESIAN_POINT ( 'NONE',  ( -1.934529033667000020, 27.70696440325999887, 1.525059720042999833 ) ) ;
#7579 = CARTESIAN_POINT ( 'NONE',  ( -2.123298534980464503, 30.87213863966240623, 0.1398201349483954581 ) ) ;
#7580 = VECTOR ( 'NONE', #6094, 1000.000000000000000 ) ;
#7581 = CARTESIAN_POINT ( 'NONE',  ( 2.255701365037127815, 11.69874888801631307, 4.259317076402555635 ) ) ;
#7582 = ORIENTED_EDGE ( 'NONE', *, *, #23836, .F. ) ;
#7583 = EDGE_CURVE ( 'NONE', #3930, #5630, #8724, .T. ) ;
#7584 = CARTESIAN_POINT ( 'NONE',  ( -4.534537486635951353, 12.33232649926562452, -1.710134897757592309 ) ) ;
#7585 = LINE ( 'NONE', #430, #17707 ) ;
#7586 = CARTESIAN_POINT ( 'NONE',  ( 1.470238514176243960, 29.51959374728719609, 1.740011424867408119 ) ) ;
#7587 = ORIENTED_EDGE ( 'NONE', *, *, #21265, .F. ) ;
#7588 = CARTESIAN_POINT ( 'NONE',  ( -23.74465998031000069, 13.93375672974000068, 0.8660254037843999608 ) ) ;
#7589 = CIRCLE ( 'NONE', #11081, 4.649999999999999467 ) ;
#7590 = CIRCLE ( 'NONE', #8776, 3.000000000000000000 ) ;
#7591 = CARTESIAN_POINT ( 'NONE',  ( 18.13612658530999866, 10.25022803218000078, -0.6090841227779000278 ) ) ;
#7592 = EDGE_CURVE ( 'NONE', #744, #16718, #22853, .T. ) ;
#7593 = CARTESIAN_POINT ( 'NONE',  ( -19.69180044273999997, -10.89175753566999916, 0.7824706121295000871 ) ) ;
#7594 = DIRECTION ( 'NONE',  ( 1.000000000000000000, 0.000000000000000000, 0.000000000000000000 ) ) ;
#7595 = CARTESIAN_POINT ( 'NONE',  ( 19.18739037306000128, 0.9675627967257999229, 10.87120185456999977 ) ) ;
#7596 = LINE ( 'NONE', #18740, #18950 ) ;
#7597 = B_SPLINE_CURVE_WITH_KNOTS ( 'NONE', 3,
 ( #23763, #12752, #20144, #13210, #15133, #7519, #2429, #11525 ),
 .UNSPECIFIED., .F., .F.,
 ( 4, 2, 2, 4 ),
 ( 0.000000000000000000, 0.2500000000000000555, 0.5000000000000001110, 1.000000000000000000 ),
 .UNSPECIFIED. ) ;
#7598 = EDGE_LOOP ( 'NONE', ( #8019, #19277 ) ) ;
#7599 = DIRECTION ( 'NONE',  ( -1.000000000000000000, 0.000000000000000000, 0.000000000000000000 ) ) ;
#7600 = CARTESIAN_POINT ( 'NONE',  ( 20.30165032445999884, 11.26076864172999947, -0.02284890567960000049 ) ) ;
#7601 = LINE ( 'NONE', #16448, #3103 ) ;
#7602 = ORIENTED_EDGE ( 'NONE', *, *, #8754, .T. ) ;
#7603 = AXIS2_PLACEMENT_3D ( 'NONE', #11817, #2241, #19194 ) ;
#7604 = CARTESIAN_POINT ( 'NONE',  ( -2.649999999999999911, 28.00000000000000000, 0.000000000000000000 ) ) ;
#7605 = CARTESIAN_POINT ( 'NONE',  ( 24.49999999999999289, 5.386536742071421635, 8.691140576888541247 ) ) ;
#7606 = B_SPLINE_CURVE_WITH_KNOTS ( 'NONE', 3,
 ( #19517, #18695, #16868, #4043, #15052, #17577, #11882, #22445, #11436 ),
 .UNSPECIFIED., .F., .F.,
 ( 4, 1, 2, 2, 4 ),
 ( 0.000000000000000000, 0.2499999999999995559, 0.3749999999999994449, 0.4999999999999993339, 1.000000000000000000 ),
 .UNSPECIFIED. ) ;
#7607 = CARTESIAN_POINT ( 'NONE',  ( 3.728119965002001823, 12.03273885954999045, 3.094591559352003252 ) ) ;
#7608 = AXIS2_PLACEMENT_3D ( 'NONE', #2056, #11027, #16701 ) ;
#7609 = CARTESIAN_POINT ( 'NONE',  ( 1.816080815948163174, 29.07698660961091264, -1.174834969488964598 ) ) ;
#7610 = CARTESIAN_POINT ( 'NONE',  ( -21.30824958319999851, -3.742314851699000133, 10.43554850291999969 ) ) ;
#7611 = ORIENTED_EDGE ( 'NONE', *, *, #13076, .F. ) ;
#7612 = AXIS2_PLACEMENT_3D ( 'NONE', #14996, #22271, #20349 ) ;
#7613 = CARTESIAN_POINT ( 'NONE',  ( 2.729128784747790970, 19.00000000000000000, 0.000000000000000000 ) ) ;
#7614 = VERTEX_POINT ( 'NONE', #19535 ) ;
#7615 = CARTESIAN_POINT ( 'NONE',  ( 2.072390219274999890, 24.98629352328999786, 1.114832866323000271 ) ) ;
#7616 = EDGE_CURVE ( 'NONE', #8416, #17203, #1238, .T. ) ;
#7617 = CARTESIAN_POINT ( 'NONE',  ( 2.500000000000001776, 28.38333333333333997, 0.3272492347489265874 ) ) ;
#7618 = CARTESIAN_POINT ( 'NONE',  ( 0.4658180156273000194, 28.71799822780999989, 2.070238309910999774 ) ) ;
#7619 = DIRECTION ( 'NONE',  ( 0.000000000000000000, -1.000000000000000000, 0.000000000000000000 ) ) ;
#7620 = EDGE_CURVE ( 'NONE', #14835, #18791, #14198, .T. ) ;
#7621 = DIRECTION ( 'NONE',  ( 0.8284926070883130711, -0.5600000000000090461, 0.000000000000000000 ) ) ;
#7622 = CARTESIAN_POINT ( 'NONE',  ( 0.000000000000000000, 1.224646799146999965E-14, 0.000000000000000000 ) ) ;
#7623 = CARTESIAN_POINT ( 'NONE',  ( 17.28506424931000041, -8.106780832215999766, 7.067619055798999739 ) ) ;
#7624 =( NAMED_UNIT ( * ) PLANE_ANGLE_UNIT ( ) SI_UNIT ( $, .RADIAN. ) );
#7625 = CARTESIAN_POINT ( 'NONE',  ( -17.83004450757999848, 9.857337362280999216, 3.100493417357999881 ) ) ;
#7626 = AXIS2_PLACEMENT_3D ( 'NONE', #9706, #7889, #5831 ) ;
#7627 = CARTESIAN_POINT ( 'NONE',  ( 0.000000000000000000, 18.50000000000000000, 0.000000000000000000 ) ) ;
#7628 = CARTESIAN_POINT ( 'NONE',  ( -14.50000017815840536, -0.2596243778326527973, 12.49999897408938487 ) ) ;
#7629 = VERTEX_POINT ( 'NONE', #19780 ) ;
#7630 = EDGE_CURVE ( 'NONE', #14966, #13647, #2963, .T. ) ;
#7631 = CARTESIAN_POINT ( 'NONE',  ( -19.30614371005000152, -10.53683211585999935, -0.2416866977026000118 ) ) ;
#7632 = AXIS2_PLACEMENT_3D ( 'NONE', #10535, #18039, #19742 ) ;
#7633 = B_SPLINE_CURVE_WITH_KNOTS ( 'NONE', 3,
 ( #17031, #7830, #11474, #546, #11955, #7952, #2622, #15201, #19341, #22597, #9884, #4197, #13274, #13388, #2749, #19081, #16905, #21025, #309, #7716, #8195, #21149, #20790, #4437, #15082, #11595, #22712, #10012, #18967, #2375, #17151, #22478, #672, #11828, #6123, #4317, #11709, #17272, #13515, #20913, #8077, #20669, #17402, #15447, #4079, #22832, #6246, #19207, #13629, #795, #15564, #22951, #6366, #13750, #1170, #1291, #1039, #4809, #19585, #913, #20150, #17768, #22077, #8563, #9122, #13879, #6615, #18329, #21281, #12195, #2990, #23316, #12076, #23067, #19461, #8314, #5372, #15922, #6497, #1734, #21517, #10378, #19707, #12761, #6730, #17889, #14122, #15680, #4930, #12316, #17641, #3120, #16495, #10505, #4691, #2868, #8678, #16043, #23437, #7173, #14564, #23885, #3557, #5485, #12865, #21959, #23199, #10942, #10130, #7292, #10252 ),
 .UNSPECIFIED., .F., .F.,
 ( 4, 2, 2, 2, 1, 2, 2, 2, 2, 2, 2, 2, 2, 2, 2, 2, 2, 2, 2, 2, 2, 2, 2, 2, 2, 2, 1, 2, 2, 2, 2, 2, 2, 2, 2, 2, 2, 2, 2, 2, 2, 2, 2, 2, 2, 2, 2, 2, 2, 2, 1, 2, 2, 2, 2, 2, 4 ),
 ( 0.000000000000000000, 0.01562500000000000000, 0.03125000000000000000, 0.04687500000000000000, 0.06250000000000000000, 0.07812500000000000000, 0.09375000000000000000, 0.1093750000000000000, 0.1250000000000000000, 0.1406250000000000000, 0.1562500000000000000, 0.1718750000000000000, 0.1875000000000000000, 0.2187500000000000000, 0.2500000000000000000, 0.2812500000000000000, 0.3125000000000000000, 0.3281250000000000000, 0.3437500000000000000, 0.3593750000000000000, 0.3750000000000000000, 0.3906250000000000000, 0.4062500000000000000, 0.4218750000000000000, 0.4375000000000000000, 0.4531250000000000000, 0.4687500000000000000, 0.4843750000000000000, 0.5000000000000000000, 0.5156250000000000000, 0.5312500000000000000, 0.5468750000000000000, 0.5625000000000000000, 0.5781250000000000000, 0.5937500000000000000, 0.6093750000000000000, 0.6250000000000000000, 0.6562500000000000000, 0.6875000000000000000, 0.7187500000000000000, 0.7500000000000000000, 0.7656250000000000000, 0.7812500000000000000, 0.7968750000000000000, 0.8125000000000000000, 0.8281250000000000000, 0.8437500000000000000, 0.8593750000000000000, 0.8750000000000000000, 0.8906250000000000000, 0.9062500000000000000, 0.9218750000000000000, 0.9375000000000000000, 0.9531250000000000000, 0.9687500000000000000, 0.9843750000000000000, 1.000000000000000000 ),
 .UNSPECIFIED. ) ;
#7634 = ADVANCED_FACE ( 'NONE', ( #1362 ), #10345, .F. ) ;
#7635 = CARTESIAN_POINT ( 'NONE',  ( -2.485790174642000139, 24.30225770961000009, 0.4464999199351999959 ) ) ;
#7636 = CARTESIAN_POINT ( 'NONE',  ( 14.19161095287168273, -8.300789259405844334, -6.118116098091685551 ) ) ;
#7637 = CARTESIAN_POINT ( 'NONE',  ( -18.33142920454666580, -4.603817514783774989, -7.987943630674345208 ) ) ;
#7638 = CARTESIAN_POINT ( 'NONE',  ( 24.41913593913999847, -0.1539011931813000222, 11.31195935673000008 ) ) ;
#7639 = CIRCLE ( 'NONE', #16135, 0.09999999999999939493 ) ;
#7640 = CARTESIAN_POINT ( 'NONE',  ( -2.239268392087999882, 29.94342548081000288, 1.226391958772999891 ) ) ;
#7641 = CARTESIAN_POINT ( 'NONE',  ( 14.26651023885097302, -0.3455854243710511087, 9.058464311847558292 ) ) ;
#7642 = CARTESIAN_POINT ( 'NONE',  ( 17.23562128263493776, -8.032680157772452034, 6.884423379150467426 ) ) ;
#7643 = CARTESIAN_POINT ( 'NONE',  ( 1.709999999999999964, 13.00000000000000000, -7.500000000000000000 ) ) ;
#7644 = PLANE ( 'NONE',  #2501 ) ;
#7645 = CARTESIAN_POINT ( 'NONE',  ( 12.28779254561780654, 13.65788853942738434, -1.343868873886438164 ) ) ;
#7646 = ORIENTED_EDGE ( 'NONE', *, *, #9697, .T. ) ;
#7647 = CARTESIAN_POINT ( 'NONE',  ( 1.236794719700695211, 24.50000548481460427, 2.172625763342098004 ) ) ;
#7648 = DIRECTION ( 'NONE',  ( 0.000000000000000000, 1.000000000000000000, 0.000000000000000000 ) ) ;
#7649 = AXIS2_PLACEMENT_3D ( 'NONE', #424, #9641, #20907 ) ;
#7650 = AXIS2_PLACEMENT_3D ( 'NONE', #3095, #12050, #10226 ) ;
#7651 = EDGE_LOOP ( 'NONE', ( #19957, #5207, #19886 ) ) ;
#7652 = CARTESIAN_POINT ( 'NONE',  ( -8.000000000000000000, 1.322618543078999814E-14, 0.000000000000000000 ) ) ;
#7653 = CARTESIAN_POINT ( 'NONE',  ( 24.50000000000000000, 10.82531754731000007, 6.250000000000000000 ) ) ;
#7654 = CARTESIAN_POINT ( 'NONE',  ( -3.150855693194152707, 28.10222989789001602, -2.799640769043123978 ) ) ;
#7655 = B_SPLINE_CURVE_WITH_KNOTS ( 'NONE', 3,
 ( #21631, #3897, #7645, #20370, #7400, #23558, #16281, #5825, #23674, #15018, #19816, #14358, #22417, #3230, #19931, #3349, #22178, #17996, #6842, #1401, #12970, #11167, #20599, #6966, #7516, #4009, #14900, #22291, #5706, #13093, #11288, #17880, #8667, #16033, #23425, #2426, #363, #725, #2310, #11406, #9698, #21078 ),
 .UNSPECIFIED., .F., .F.,
 ( 4, 2, 1, 2, 2, 2, 1, 2, 2, 2, 2, 2, 2, 2, 2, 1, 2, 2, 2, 1, 2, 2, 4 ),
 ( 0.000000000000000000, 0.06250000000000087430, 0.09375000000000137390, 0.1093750000000017208, 0.1250000000000020817, 0.1875000000000032196, 0.2187500000000036637, 0.2343750000000038025, 0.2500000000000039413, 0.3125000000000041633, 0.3750000000000043299, 0.5000000000000043299, 0.5625000000000044409, 0.6250000000000044409, 0.6875000000000043299, 0.7187500000000044409, 0.7343750000000045519, 0.7500000000000045519, 0.8125000000000032196, 0.8437500000000026645, 0.8593750000000024425, 0.8750000000000022204, 1.000000000000000000 ),
 .UNSPECIFIED. ) ;
#7656 = CARTESIAN_POINT ( 'NONE',  ( 18.23447124448000167, 6.119127544384999950, -9.282487988299001458 ) ) ;
#7657 = CARTESIAN_POINT ( 'NONE',  ( 0.000000000000000000, 15.04999987253367877, -4.699999872533999756 ) ) ;
#7658 = CARTESIAN_POINT ( 'NONE',  ( -0.8328668639932000906, 28.33669433610000254, 2.747163055864000114 ) ) ;
#7659 = ORIENTED_EDGE ( 'NONE', *, *, #9399, .F. ) ;
#7660 = VERTEX_POINT ( 'NONE', #10295 ) ;
#7661 = CARTESIAN_POINT ( 'NONE',  ( 0.6543697108981985089, 27.20086340285667248, -2.434931691670790599 ) ) ;
#7662 = CARTESIAN_POINT ( 'NONE',  ( 0.5338398250025285785, 6.797827069970633573, -1.670807105909973167 ) ) ;
#7663 = CARTESIAN_POINT ( 'NONE',  ( 17.79862270046333350, 8.831439506605962109, 2.665405980357957727 ) ) ;
#7664 = ORIENTED_EDGE ( 'NONE', *, *, #13868, .T. ) ;
#7665 = CARTESIAN_POINT ( 'NONE',  ( -14.33281118273302290, 8.249344442837845293, 10.71171629587128926 ) ) ;
#7666 = CARTESIAN_POINT ( 'NONE',  ( 19.44079720308818082, -8.366211633341873011, -6.347735393923803038 ) ) ;
#7667 = FACE_OUTER_BOUND ( 'NONE', #1743, .T. ) ;
#7668 = CARTESIAN_POINT ( 'NONE',  ( 15.58037287370735946, -6.899987183789440870, 7.711731525822442812 ) ) ;
#7669 = CIRCLE ( 'NONE', #7279, 9.017718320138000010 ) ;
#7670 = CARTESIAN_POINT ( 'NONE',  ( -15.73688287099999883, -7.860281848462999932, 7.750493481497999326 ) ) ;
#7671 = CARTESIAN_POINT ( 'NONE',  ( -1.822202359507000047, 29.26374338476000148, 1.219654227816000081 ) ) ;
#7672 = CARTESIAN_POINT ( 'NONE',  ( -19.33347310582000134, -11.41588003357999881, 0.8201876405482001475 ) ) ;
#7673 = CIRCLE ( 'NONE', #708, 4.000000000000000000 ) ;
#7674 = CARTESIAN_POINT ( 'NONE',  ( 1.439338077355937662, 29.69654873358969027, 1.610574062856036992 ) ) ;
#7675 = ORIENTED_EDGE ( 'NONE', *, *, #6119, .T. ) ;
#7676 = CARTESIAN_POINT ( 'NONE',  ( 2.083478469512000331, 25.85240551230000250, -0.3289914792577999791 ) ) ;
#7677 = LINE ( 'NONE', #23004, #17792 ) ;
#7678 = DIRECTION ( 'NONE',  ( 0.000000000000000000, 0.000000000000000000, -1.000000000000000000 ) ) ;
#7679 = VECTOR ( 'NONE', #17009, 1000.000000000000000 ) ;
#7680 = VERTEX_POINT ( 'NONE', #14290 ) ;
#7681 = CARTESIAN_POINT ( 'NONE',  ( 24.35625626386766740, -3.237027092068850198, 12.50000000000000000 ) ) ;
#7682 = B_SPLINE_CURVE_WITH_KNOTS ( 'NONE', 3,
 ( #14799, #7903, #22662, #20866, #2446, #9839, #12989, #22195, #5608, #20512, #9361, #22311, #5727, #16857 ),
 .UNSPECIFIED., .F., .F.,
 ( 4, 2, 2, 2, 2, 2, 4 ),
 ( 0.000000000000000000, 0.2500000000000001665, 0.3750000000000000555, 0.5000000000000000000, 0.6250000000000000000, 0.7499999999999998890, 1.000000000000000000 ),
 .UNSPECIFIED. ) ;
#7683 = CARTESIAN_POINT ( 'NONE',  ( 13.50000000000000000, 2.048741218006000064, 10.08990150394999930 ) ) ;
#7684 = CARTESIAN_POINT ( 'NONE',  ( 12.92793875730999886, -7.038709952280000515, 5.788476981990000603 ) ) ;
#7685 = ORIENTED_EDGE ( 'NONE', *, *, #16471, .F. ) ;
#7686 = CARTESIAN_POINT ( 'NONE',  ( -6.145346148252000873, 15.63690921201999018, -1.260321238843998604 ) ) ;
#7687 = CARTESIAN_POINT ( 'NONE',  ( 24.28455689590275668, -12.82067141883539918, 2.793945715430803389 ) ) ;
#7688 = AXIS2_PLACEMENT_3D ( 'NONE', #23178, #6596, #21006 ) ;
#7689 = ORIENTED_EDGE ( 'NONE', *, *, #17956, .T. ) ;
#7690 = DIRECTION ( 'NONE',  ( -0.8193292504149890521, 0.5733232765328929448, 2.256055603357969935E-11 ) ) ;
#7691 = LINE ( 'NONE', #16882, #11295 ) ;
#7692 = CARTESIAN_POINT ( 'NONE',  ( 4.720281943117000445, 12.53503215193000209, -0.1499393658648999206 ) ) ;
#7693 = VECTOR ( 'NONE', #19256, 1000.000000000000114 ) ;
#7694 = CARTESIAN_POINT ( 'NONE',  ( -20.37005317997999754, -8.126137106287000478, 5.051193361354000544 ) ) ;
#7695 = CARTESIAN_POINT ( 'NONE',  ( -14.47125383376828367, 9.790219516183384485, -8.042794959416264433 ) ) ;
#7696 = CLOSED_SHELL ( 'NONE', ( #23822, #22265, #12472, #11317, #1230, #6444 ) ) ;
#7697 = DIRECTION ( 'NONE',  ( 0.000000000000000000, 1.000000000000000000, 0.000000000000000000 ) ) ;
#7698 = DIRECTION ( 'NONE',  ( 1.000000000000000000, 0.000000000000000000, 0.000000000000000000 ) ) ;
#7699 = AXIS2_PLACEMENT_3D ( 'NONE', #23122, #10671, #19761 ) ;
#7700 = CARTESIAN_POINT ( 'NONE',  ( 1.678813317411953498, 26.50000000000001066, -3.649538832790644616 ) ) ;
#7701 = DIRECTION ( 'NONE',  ( -1.000000000000000000, 0.000000000000000000, 0.000000000000000000 ) ) ;
#7702 = EDGE_CURVE ( 'NONE', #23303, #17082, #11467, .T. ) ;
#7703 = CARTESIAN_POINT ( 'NONE',  ( -0.1404717678206177378, 30.39552274579631685, 2.155312933377941498 ) ) ;
#7704 = ORIENTED_EDGE ( 'NONE', *, *, #21015, .T. ) ;
#7705 = CARTESIAN_POINT ( 'NONE',  ( -17.61928743917333762, 7.295792109983556095, -5.606682590099613783 ) ) ;
#7706 = DIRECTION ( 'NONE',  ( 0.000000000000000000, 1.000000000000000000, 0.000000000000000000 ) ) ;
#7707 = CARTESIAN_POINT ( 'NONE',  ( -2.771665969827710185, 13.06403465582575052, -6.137156239621617715 ) ) ;
#7708 = CARTESIAN_POINT ( 'NONE',  ( 2.184465970885649089, 27.76753006952332825, 1.259047450927240241 ) ) ;
#7709 = CIRCLE ( 'NONE', #22416, 2.100000000000000089 ) ;
#7710 = CARTESIAN_POINT ( 'NONE',  ( -23.72355754295171693, 10.26472423533547484, 2.601420961443067448 ) ) ;
#7711 = CARTESIAN_POINT ( 'NONE',  ( -0.2414528406811999872, 26.63446440325999731, -2.451511826319000331 ) ) ;
#7712 = CIRCLE ( 'NONE', #18930, 14.43375672973999890 ) ;
#7713 = AXIS2_PLACEMENT_3D ( 'NONE', #14631, #18047, #18508 ) ;
#7714 = CARTESIAN_POINT ( 'NONE',  ( -0.8491321808595133636, 28.10222989789001957, 4.128541458487867466 ) ) ;
#7715 = ORIENTED_EDGE ( 'NONE', *, *, #7761, .F. ) ;
#7716 = CARTESIAN_POINT ( 'NONE',  ( -18.54960927350814970, 8.133714014779581447, -6.579685461590351281 ) ) ;
#7717 = EDGE_CURVE ( 'NONE', #18727, #10512, #22990, .T. ) ;
#7718 = CARTESIAN_POINT ( 'NONE',  ( 23.99062354302999722, -7.716878364870000340, -11.63397459621999985 ) ) ;
#7719 = CARTESIAN_POINT ( 'NONE',  ( 4.834780805419000238, 12.45065217972999960, 0.000000000000000000 ) ) ;
#7720 = VERTEX_POINT ( 'NONE', #10175 ) ;
#7721 = CARTESIAN_POINT ( 'NONE',  ( -1.779764907139927077, 26.49975665830813298, 1.755621799651315262 ) ) ;
#7722 = CARTESIAN_POINT ( 'NONE',  ( 18.57487658530999752, 1.133029877492999882, 10.21722326572000128 ) ) ;
#7723 = AXIS2_PLACEMENT_3D ( 'NONE', #4435, #13272, #11472 ) ;
#7724 = CARTESIAN_POINT ( 'NONE',  ( -18.81322861345999797, 5.160499379352000204, -10.20084603521000055 ) ) ;
#7725 = CARTESIAN_POINT ( 'NONE',  ( 22.79641666666664790, 9.015317850787624820, -2.422929696547522660 ) ) ;
#7726 = CARTESIAN_POINT ( 'NONE',  ( 18.98426537306000128, 7.768735744027000401, 7.659878704847000286 ) ) ;
#7727 = CARTESIAN_POINT ( 'NONE',  ( -0.6074916215089999350, 30.83999999999999986, -2.072813047478000215 ) ) ;
#7728 = DIRECTION ( 'NONE',  ( 0.000000000000000000, 1.000000000000000000, 5.996565258237018052E-10 ) ) ;
#7729 = CARTESIAN_POINT ( 'NONE',  ( 20.13606306023999792, -7.887424479675998690, -6.464295009536999537 ) ) ;
#7730 = EDGE_CURVE ( 'NONE', #7738, #16445, #22666, .T. ) ;
#7731 = CARTESIAN_POINT ( 'NONE',  ( 4.000000000000000000, 24.80000000000000426, -2.309401076759000304 ) ) ;
#7732 = ORIENTED_EDGE ( 'NONE', *, *, #15763, .T. ) ;
#7733 = CARTESIAN_POINT ( 'NONE',  ( 11.73400169467000076, -6.466195830854000626, -6.710731160583000232 ) ) ;
#7734 = LINE ( 'NONE', #11012, #21514 ) ;
#7735 = CARTESIAN_POINT ( 'NONE',  ( -4.021760009708001959, 12.12704307397999770, 2.703375033665003091 ) ) ;
#7736 = DIRECTION ( 'NONE',  ( 0.000000000000000000, 1.000000000000000000, 0.000000000000000000 ) ) ;
#7737 = CARTESIAN_POINT ( 'NONE',  ( -24.72040429820999918, -9.265427320653000010, -5.484610141081000201 ) ) ;
#7738 = VERTEX_POINT ( 'NONE', #19503 ) ;
#7739 = CARTESIAN_POINT ( 'NONE',  ( -1.059324317249869862, 23.72850810831080537, 1.979001141744386016 ) ) ;
#7740 = ORIENTED_EDGE ( 'NONE', *, *, #12210, .T. ) ;
#7741 = CARTESIAN_POINT ( 'NONE',  ( -0.5893288717795999165, 23.58034700824000041, -2.005185021572999826 ) ) ;
#7742 = CARTESIAN_POINT ( 'NONE',  ( 4.811488400566996226, 14.48490630412999991, 3.723044770969999639 ) ) ;
#7744 = EDGE_CURVE ( 'NONE', #13227, #20019, #1011, .T. ) ;
#7743 = CARTESIAN_POINT ( 'NONE',  ( 2.169172474974999876, 25.72799822781000145, -0.6576354733792000307 ) ) ;
#7745 = CARTESIAN_POINT ( 'NONE',  ( 0.000000000000000000, 24.49999999999999645, 0.000000000000000000 ) ) ;
#7746 = CARTESIAN_POINT ( 'NONE',  ( -4.544340308300998998, 13.49051417780999884, -5.132142894851999593 ) ) ;
#7747 = CARTESIAN_POINT ( 'NONE',  ( 14.54287674931000041, 7.516034287427999949, -7.591774476630000379 ) ) ;
#7748 = CARTESIAN_POINT ( 'NONE',  ( -17.01752311569999776, -10.30819550402000040, 0.2320531645540999943 ) ) ;
#7749 = CARTESIAN_POINT ( 'NONE',  ( 0.000000000000000000, 13.04999996922999905, 0.000000000000000000 ) ) ;
#7750 = EDGE_CURVE ( 'NONE', #2709, #3157, #12753, .T. ) ;
#7751 = CARTESIAN_POINT ( 'NONE',  ( -11.00000000000000000, 1.359357947053999856E-14, 0.000000000000000000 ) ) ;
#7752 = ORIENTED_EDGE ( 'NONE', *, *, #19016, .F. ) ;
#7753 = CARTESIAN_POINT ( 'NONE',  ( -4.000000000000000000, 30.00000000000000000, 0.000000000000000000 ) ) ;
#7754 = CARTESIAN_POINT ( 'NONE',  ( -1.025360869613999748, 24.32490530784000171, 2.515071452785000439 ) ) ;
#7755 = CARTESIAN_POINT ( 'NONE',  ( 13.68447321782882220, -4.482739838237562502, 9.298704708330065571 ) ) ;
#7756 = DIRECTION ( 'NONE',  ( -0.8193292504149890521, -0.5733232765328929448, -2.256442838868970230E-11 ) ) ;
#7757 = CARTESIAN_POINT ( 'NONE',  ( 22.66677564524290744, 35.31760589360604996, -6.000000000000000000 ) ) ;
#7758 = ADVANCED_FACE ( 'NONE', ( #4851 ), #1083, .T. ) ;
#7759 = CARTESIAN_POINT ( 'NONE',  ( -2.179821160686999715, 29.00990996801999700, -1.329187652093999805 ) ) ;
#7760 = CARTESIAN_POINT ( 'NONE',  ( 14.43361646158383849, -5.276216224350072537, 7.393200072960158131 ) ) ;
#7761 = EDGE_CURVE ( 'NONE', #20998, #7342, #10310, .T. ) ;
#7762 = CARTESIAN_POINT ( 'NONE',  ( 24.50000000000000000, 10.82531754731000007, -6.250000000000000000 ) ) ;
#7763 = CARTESIAN_POINT ( 'NONE',  ( 0.000000000000000000, 15.04999987253367877, 0.000000000000000000 ) ) ;
#7764 = DIRECTION ( 'NONE',  ( -1.000000000000000000, 0.000000000000000000, 0.000000000000000000 ) ) ;
#7765 = ORIENTED_EDGE ( 'NONE', *, *, #16750, .F. ) ;
#7766 = CARTESIAN_POINT ( 'NONE',  ( 0.9744765624120647063, 29.91693820796410463, -4.056187847889995091 ) ) ;
#7767 = ORIENTED_EDGE ( 'NONE', *, *, #3900, .F. ) ;
#7768 = CARTESIAN_POINT ( 'NONE',  ( -10.25814758309999952, 7.142857142857000241, 0.000000000000000000 ) ) ;
#7769 = CARTESIAN_POINT ( 'NONE',  ( 24.07420734439588372, 7.985988878874604069, 11.16786151310754960 ) ) ;
#7770 = EDGE_CURVE ( 'NONE', #19823, #3092, #7803, .T. ) ;
#7771 = DIRECTION ( 'NONE',  ( 0.000000000000000000, -1.000000000000000000, 0.000000000000000000 ) ) ;
#7772 = ORIENTED_EDGE ( 'NONE', *, *, #19152, .F. ) ;
#7773 = CARTESIAN_POINT ( 'NONE',  ( 15.34725687895999791, -0.07841823125676000705, 11.03857397622999947 ) ) ;
#7774 = AXIS2_PLACEMENT_3D ( 'NONE', #429, #4564, #9650 ) ;
#7775 = CARTESIAN_POINT ( 'NONE',  ( 0.000000000000000000, 15.09999999999999964, 0.000000000000000000 ) ) ;
#7776 = CARTESIAN_POINT ( 'NONE',  ( -2.656868203660999850, 27.46712896666999626, -0.2616786785207999566 ) ) ;
#7777 = ORIENTED_EDGE ( 'NONE', *, *, #17181, .F. ) ;
#7778 = ORIENTED_EDGE ( 'NONE', *, *, #6046, .F. ) ;
#7779 = CARTESIAN_POINT ( 'NONE',  ( -14.00000000000000178, 3.538282677300232937, -8.592818941365493401 ) ) ;
#7780 = CARTESIAN_POINT ( 'NONE',  ( -11.10888721168999993, -1.831216772004999882, -15.46077555675999982 ) ) ;
#7781 = CARTESIAN_POINT ( 'NONE',  ( 1.693959225995342432, 6.986248014536463380, -0.4526555866337934608 ) ) ;
#7782 = CARTESIAN_POINT ( 'NONE',  ( -24.33938584176036102, -9.417644943810280722, -8.688014043590282398 ) ) ;
#7783 = ORIENTED_EDGE ( 'NONE', *, *, #7007, .F. ) ;
#7784 = CARTESIAN_POINT ( 'NONE',  ( -20.11677904293000196, -5.490517660549000034, -7.911588380172000612 ) ) ;
#7785 = CARTESIAN_POINT ( 'NONE',  ( -14.47826289458183702, 9.918718668892536172, 7.820280362110097805 ) ) ;
#7786 = CARTESIAN_POINT ( 'NONE',  ( 6.147856022268394227, 14.14629814091362725, 0.2181625506079420684 ) ) ;
#7787 = CARTESIAN_POINT ( 'NONE',  ( 15.84992198554521003, -10.31145118159957441, -0.9790302175844434185 ) ) ;
#7788 = CARTESIAN_POINT ( 'NONE',  ( -17.69013761820000141, -8.094509216140998831, 7.584009060629000487 ) ) ;
#7789 = EDGE_CURVE ( 'NONE', #20876, #15884, #1425, .T. ) ;
#7790 = CARTESIAN_POINT ( 'NONE',  ( -2.192791562915999748, 30.85570112213000016, 0.6001452317431000827 ) ) ;
#7791 = CARTESIAN_POINT ( 'NONE',  ( -19.13034275784999849, -9.231395905450000328, -6.758791263612999423 ) ) ;
#7792 = CARTESIAN_POINT ( 'NONE',  ( 0.4770046633850718032, 29.63206295647701438, 2.106562789758566367 ) ) ;
#7793 = EDGE_LOOP ( 'NONE', ( #2888, #17047, #22717, #10824, #21960 ) ) ;
#7794 = CARTESIAN_POINT ( 'NONE',  ( -1.286689466012000072, 24.54815262634000206, 1.965122128918000088 ) ) ;
#7795 = DIRECTION ( 'NONE',  ( 0.000000000000000000, 1.000000000000000000, 0.000000000000000000 ) ) ;
#7796 = CARTESIAN_POINT ( 'NONE',  ( -19.44055257232857770, -10.47407731232025085, -0.6087492459073309270 ) ) ;
#7797 = ORIENTED_EDGE ( 'NONE', *, *, #8518, .F. ) ;
#7798 = CARTESIAN_POINT ( 'NONE',  ( -5.470390416431995639, 16.57655522344998644, 3.044249783594998426 ) ) ;
#7799 = ADVANCED_FACE ( 'NONE', ( #19861 ), #6895, .T. ) ;
#7800 = PLANE ( 'NONE',  #13381 ) ;
#7801 = CARTESIAN_POINT ( 'NONE',  ( 16.90312642131000231, -9.179335210403001710, 3.217155551743000164 ) ) ;
#7802 = ORIENTED_EDGE ( 'NONE', *, *, #23769, .F. ) ;
#7803 = B_SPLINE_CURVE_WITH_KNOTS ( 'NONE', 3,
 ( #14045, #1208, #6536, #12239, #13920, #8237, #21438, #19626, #21193, #17813, #8600, #21316, #15962, #1334, #23356, #6773, #14166, #4976 ),
 .UNSPECIFIED., .F., .F.,
 ( 4, 2, 2, 2, 2, 2, 2, 2, 4 ),
 ( 0.000000000000000000, 0.1250000000000000000, 0.2500000000000000000, 0.3750000000000000555, 0.5000000000000000000, 0.6250000000000000000, 0.7500000000000000000, 0.8750000000000000000, 1.000000000000000000 ),
 .UNSPECIFIED. ) ;
#7804 = CARTESIAN_POINT ( 'NONE',  ( -6.100000173032002593, 16.42883599709998776, -1.007191989855000358 ) ) ;
#7805 = DIRECTION ( 'NONE',  ( -0.7071067811865465735, -0.7071067811865465735, -5.144932280347337440E-08 ) ) ;
#7806 = AXIS2_PLACEMENT_3D ( 'NONE', #605, #8006, #15381 ) ;
#7807 = ORIENTED_EDGE ( 'NONE', *, *, #17535, .F. ) ;
#7808 = FACE_OUTER_BOUND ( 'NONE', #15679, .T. ) ;
#7809 = CARTESIAN_POINT ( 'NONE',  ( -12.48828895470000155, 6.965227931770999525, -5.686587078224999203 ) ) ;
#7810 = CARTESIAN_POINT ( 'NONE',  ( -4.686906630868004520, 12.59381172247999636, 0.7274896323178006163 ) ) ;
#7811 = CARTESIAN_POINT ( 'NONE',  ( 24.50000000000000000, 12.49999999999416822, 0.000000000000000000 ) ) ;
#7812 = CARTESIAN_POINT ( 'NONE',  ( 11.99999999999999822, -4.176273271679210808, -8.652910017623161920 ) ) ;
#7813 = CARTESIAN_POINT ( 'NONE',  ( -10.90000000000000036, 10.50000000000000000, 1.712914282636999961E-09 ) ) ;
#7814 = FACE_BOUND ( 'NONE', #16123, .T. ) ;
#7815 = CARTESIAN_POINT ( 'NONE',  ( -3.064125534931649852, 26.41068681084918879, -2.849728451093326065 ) ) ;
#7816 = CIRCLE ( 'NONE', #1638, 7.000000000000000000 ) ;
#7817 =( NAMED_UNIT ( * ) SI_UNIT ( $, .STERADIAN. ) SOLID_ANGLE_UNIT ( ) );
#7818 = CARTESIAN_POINT ( 'NONE',  ( 0.3272492347489341924, 28.01753006952333536, -2.500000000000000888 ) ) ;
#7819 =( BOUNDED_SURFACE ( )  B_SPLINE_SURFACE ( 3, 3, ( 
 ( #21292, #6377, #13889, #10390, #17652, #2761 ),
 ( #19720, #10264, #4704, #12089, #8452, #6741 ),
 ( #23450, #15819, #19472, #15690, #8325, #14136 ),
 ( #23081, #19834, #23210, #21529, #6626, #4944 ) ),
 .UNSPECIFIED., .F., .F., .T. ) 
 B_SPLINE_SURFACE_WITH_KNOTS ( ( 4, 4 ),
 ( 4, 1, 1, 4 ),
 ( 0.000000000000000000, 1.000000000000000000 ),
 ( 0.01136608918049999972, 0.01481517776244999952, 0.02900961618256999927, 0.03401603006026000103 ),
 .UNSPECIFIED. ) 
 GEOMETRIC_REPRESENTATION_ITEM ( )  RATIONAL_B_SPLINE_SURFACE ( (
 ( 1.047527064320000090, 1.047527064320000090, 1.047527064320000090, 1.047527064320000090, 1.047527064320000090, 1.047527064320000090),
 ( 0.9841576452265000663, 0.9841576452265000663, 0.9841576452265000663, 0.9841576452265000663, 0.9841576452265000663, 0.9841576452265000663),
 ( 0.9841576452265000663, 0.9841576452265000663, 0.9841576452265000663, 0.9841576452265000663, 0.9841576452265000663, 0.9841576452265000663),
 ( 1.047527064320000090, 1.047527064320000090, 1.047527064320000090, 1.047527064320000090, 1.047527064320000090, 1.047527064320000090) ) ) 
 REPRESENTATION_ITEM ( '' )  SURFACE ( )  );
#7820 = CARTESIAN_POINT ( 'NONE',  ( 2.149588097096659656, 30.59149455840149656, 0.2106377642020627605 ) ) ;
#7821 = EDGE_LOOP ( 'NONE', ( #4138, #17335 ) ) ;
#7822 = CARTESIAN_POINT ( 'NONE',  ( -18.29953743917332787, -9.140883910219043784, -1.196665853474646823 ) ) ;
#7823 = CARTESIAN_POINT ( 'NONE',  ( 1.547176311163561024, 12.88373697569958232, -6.507343160275748772 ) ) ;
#7824 = B_SPLINE_CURVE_WITH_KNOTS ( 'NONE', 3,
 ( #12861, #1964, #9468, #20261, #11410, #369, #16844, #9348, #11052, #18435, #15135, #247, #5366, #1846, #12756, #3783, #16722, #10938 ),
 .UNSPECIFIED., .F., .F.,
 ( 4, 2, 2, 2, 2, 2, 2, 2, 4 ),
 ( 0.000000000000000000, 0.1250000000000000555, 0.2500000000000000555, 0.3750000000000000555, 0.5000000000000000000, 0.6249999999999998890, 0.7500000000000000000, 0.8750000000000000000, 1.000000000000000000 ),
 .UNSPECIFIED. ) ;
#7825 = CARTESIAN_POINT ( 'NONE',  ( -22.59894979209085619, -5.689294951490594165, -8.900361714202414731 ) ) ;
#7826 = CARTESIAN_POINT ( 'NONE',  ( -0.3375125786564999730, 27.80446440325999902, 2.440142399906000126 ) ) ;
#7827 = AXIS2_PLACEMENT_3D ( 'NONE', #9718, #14913, #7414 ) ;
#7828 = DIRECTION ( 'NONE',  ( 0.000000000000000000, 0.000000000000000000, 1.000000000000000000 ) ) ;
#7829 = ORIENTED_EDGE ( 'NONE', *, *, #14686, .T. ) ;
#7830 = CARTESIAN_POINT ( 'NONE',  ( -19.33112391592212020, -10.16448900941933253, 2.551422195813828342 ) ) ;
#7831 = LINE ( 'NONE', #18968, #9189 ) ;
#7832 = DIRECTION ( 'NONE',  ( 0.000000000000000000, 0.000000000000000000, -1.000000000000000000 ) ) ;
#7833 = CARTESIAN_POINT ( 'NONE',  ( -10.90000000000000036, 1.358133300253999998E-14, 0.000000000000000000 ) ) ;
#7834 = EDGE_CURVE ( 'NONE', #6411, #14911, #14182, .T. ) ;
#7835 = ORIENTED_EDGE ( 'NONE', *, *, #17108, .T. ) ;
#7836 = DIRECTION ( 'NONE',  ( -1.000000000000000000, 0.000000000000000000, 0.000000000000000000 ) ) ;
#7837 = CARTESIAN_POINT ( 'NONE',  ( 14.65256424931000190, 9.798150841947000700, -4.264230833847999946 ) ) ;
#7838 = CARTESIAN_POINT ( 'NONE',  ( 0.000000000000000000, 7.000000000000000000, -1.399999999999999911 ) ) ;
#7839 = CARTESIAN_POINT ( 'NONE',  ( 22.72083333333331367, 8.086270432886472292, -4.660780108671074728 ) ) ;
#7840 = B_SPLINE_CURVE_WITH_KNOTS ( 'NONE', 3,
 ( #17613, #23167, #13971, #2959, #1733, #20149, #10706, #14341, #16010, #18099, #16134, #19912 ),
 .UNSPECIFIED., .F., .F.,
 ( 4, 1, 1, 1, 1, 2, 2, 4 ),
 ( 0.000000000000000000, 0.2500000000000007772, 0.3750000000000009437, 0.4375000000000009992, 0.4687500000000009437, 0.4843750000000008327, 0.5000000000000006661, 1.000000000000000000 ),
 .UNSPECIFIED. ) ;
#7841 = CARTESIAN_POINT ( 'NONE',  ( 16.74989037305999773, 8.450119865360001370, -6.801369492786998983 ) ) ;
#7842 = CARTESIAN_POINT ( 'NONE',  ( -1.938959741890676325, 30.88393747333224937, -0.8889222898575229737 ) ) ;
#7843 = VECTOR ( 'NONE', #8150, 1000.000000000000000 ) ;
#7844 = DIRECTION ( 'NONE',  ( 0.000000000000000000, -1.000000000000000000, 0.000000000000000000 ) ) ;
#7845 = CARTESIAN_POINT ( 'NONE',  ( 24.12539877769000185, -5.296127428040000140, -8.219271541286000016 ) ) ;
#7846 = B_SPLINE_SURFACE_WITH_KNOTS ( 'NONE', 3, 3, ( 
 ( #19324, #11814, #12510, #5127, #8180, #23645, #21134, #6353, #18082, #18208, #15664, #7052, #12627, #19191, #2601, #13736, #17382, #19895, #4675, #780, #4545, #3433, #12060, #14434, #23185, #15549, #9993, #21830, #22936, #21264, #17504, #1609, #2733, #14329, #3312 ),
 ( #10692, #11939, #10115, #10818, #898, #1488, #8300, #8882, #16365, #21717, #6478, #13861, #20012, #19446, #2854, #5242, #15793, #10236, #8995, #17628, #23754, #1022, #8425, #6933, #16252, #7158, #21011, #4423, #5699, #13085, #4003, #10928, #11400, #14668, #18769 ),
 ( #22062, #1835, #9221, #7638, #16478, #21943, #20485, #2179, #9572, #1953, #18660, #5471, #5353, #16958, #16601, #357, #18314, #16832, #22410, #16711, #3892, #12743, #1716, #14548, #11283, #20136, #9339, #3544, #5819, #9105, #11, #7394, #3771, #23868, #7275 ),
 ( #13201, #12966, #12853, #2066, #20249, #20594, #14777, #235, #3655, #5584, #22284, #11041, #22173, #20362, #18424, #11160, #18546, #123, #9458, #7510, #14893, #12000, #5929, #21195, #4249, #471, #2669, #11638, #6045, #13314, #17445, #19384, #20837, #11753, #7874 ) ),
 .UNSPECIFIED., .F., .F., .F.,
 ( 4, 4 ),
 ( 4, 1, 1, 1, 1, 1, 1, 1, 1, 1, 1, 1, 1, 1, 1, 1, 1, 1, 1, 1, 1, 1, 1, 1, 1, 1, 1, 1, 1, 1, 1, 1, 4 ),
 ( -0.6000240009599999702, 1.600024000959999970 ),
 ( 0.1465850610777999774, 0.1737772037394999802, 0.2009693464012999864, 0.2281614890629999892, 0.2553536317247000476, 0.2825457743865000260, 0.3097379170481999733, 0.3369300597100000072, 0.3641222023717000100, 0.3913143450334000129, 0.4185064876951999913, 0.4456986303568999941, 0.4728907730185999969, 0.5000829156803999753, 0.5272750583420999781, 0.5544672010039000121, 0.5816593436656000149, 0.6088514863273000177, 0.6360436289891000516, 0.6632357716507999434, 0.6904279143125000573, 0.7176200569742999802, 0.7448121996359999830, 0.7720043422976999858, 0.7991964849595000198, 0.8263886276212000226, 0.8535807702829999455, 0.8807729129446999483, 0.9079650556064000622, 0.9351571982681999851, 0.9623493409299000989, 0.9895414835915999907, 1.016733626253000011 ),
 .UNSPECIFIED. ) ;
#7847 = CARTESIAN_POINT ( 'NONE',  ( 4.000000000000000000, 29.69999999999999929, 2.309401076759000304 ) ) ;
#7848 = ORIENTED_EDGE ( 'NONE', *, *, #15366, .F. ) ;
#7849 = DIRECTION ( 'NONE',  ( 0.000000000000000000, 0.000000000000000000, -1.000000000000000000 ) ) ;
#7850 = CARTESIAN_POINT ( 'NONE',  ( -1.812210406530999851, 27.25956776952000027, 1.960438172911999954 ) ) ;
#7851 = CARTESIAN_POINT ( 'NONE',  ( 0.8254538522422999458, 11.46557405689998710, 4.793380782510001659 ) ) ;
#7852 = CARTESIAN_POINT ( 'NONE',  ( 2.056388550342119981, 28.96414759127528171, 0.6606570080441251935 ) ) ;
#7853 = CARTESIAN_POINT ( 'NONE',  ( -19.95111026805999899, 7.370637296965999674, 8.231908711352000196 ) ) ;
#7854 = ORIENTED_EDGE ( 'NONE', *, *, #14726, .T. ) ;
#7855 = CARTESIAN_POINT ( 'NONE',  ( -4.750000000000000000, 24.29999999999999716, 0.000000000000000000 ) ) ;
#7856 = ORIENTED_EDGE ( 'NONE', *, *, #2301, .F. ) ;
#7857 = DIRECTION ( 'NONE',  ( 0.000000000000000000, 1.000000000000000000, 0.000000000000000000 ) ) ;
#7858 = CARTESIAN_POINT ( 'NONE',  ( -0.6273549637530023704, 11.57490430900510248, 4.750118582288012981 ) ) ;
#7859 = CARTESIAN_POINT ( 'NONE',  ( -1.538852087555999892, 26.99549822780999975, 1.664720809480999986 ) ) ;
#7860 = CARTESIAN_POINT ( 'NONE',  ( -3.793527413694002703, 13.19029577252999097, 5.954828092150002306 ) ) ;
#7861 = CARTESIAN_POINT ( 'NONE',  ( -1.795213620510333064, 26.49800875556814006, 1.739922323311954511 ) ) ;
#7862 = CARTESIAN_POINT ( 'NONE',  ( 16.95600174931000126, 3.031816831187000183, 10.30986099653000032 ) ) ;
#7863 = EDGE_CURVE ( 'NONE', #3365, #14211, #5758, .T. ) ;
#7864 = CARTESIAN_POINT ( 'NONE',  ( -16.40813207178999988, 5.092047131649000136, -8.946165747030999427 ) ) ;
#7865 = CARTESIAN_POINT ( 'NONE',  ( 14.68293875730999964, -5.746474821545000111, 7.132383943660999925 ) ) ;
#7866 = VECTOR ( 'NONE', #13112, 1000.000000000000227 ) ;
#7867 = CARTESIAN_POINT ( 'NONE',  ( -14.47826287373907128, -1.813202974726752625, 12.50000251923937000 ) ) ;
#7868 = EDGE_LOOP ( 'NONE', ( #12549, #8167 ) ) ;
#7869 = CARTESIAN_POINT ( 'NONE',  ( -1.109830502371000005, 31.11496756662999985, -2.398385042689000102 ) ) ;
#7870 = CARTESIAN_POINT ( 'NONE',  ( -2.673271556775000057, 24.19682307903999785, 0.4801754984155000017 ) ) ;
#7871 = CARTESIAN_POINT ( 'NONE',  ( 14.28671968858128771, -5.872878552574734456, -8.509277291877729965 ) ) ;
#7872 = ORIENTED_EDGE ( 'NONE', *, *, #23627, .F. ) ;
#7873 = CARTESIAN_POINT ( 'NONE',  ( -4.752114190998003806, 13.48439568903999053, -5.196290741126996515 ) ) ;
#7874 = CARTESIAN_POINT ( 'NONE',  ( 19.05934864702000198, 2.169758708643000134, 10.21046665093999906 ) ) ;
#7875 = CARTESIAN_POINT ( 'NONE',  ( -2.576169063563999551, 30.60395229662999839, 0.6192135579617999985 ) ) ;
#7876 = EDGE_CURVE ( 'NONE', #12335, #9818, #22580, .T. ) ;
#7877 = CARTESIAN_POINT ( 'NONE',  ( 11.85409292833783468, 4.507814091383394839, 12.50002426122780186 ) ) ;
#7878 = DIRECTION ( 'NONE',  ( 1.000000000000000000, 0.000000000000000000, 0.000000000000000000 ) ) ;
#7879 = DIRECTION ( 'NONE',  ( 0.000000000000000000, -1.000000000000000000, 0.000000000000000000 ) ) ;
#7880 = CARTESIAN_POINT ( 'NONE',  ( -6.149942199219999850, 16.31029674404999952, 1.000000882129999935 ) ) ;
#7881 = CARTESIAN_POINT ( 'NONE',  ( -5.625000000000000000, 22.00000000000000000, 0.000000000000000000 ) ) ;
#7882 = ORIENTED_EDGE ( 'NONE', *, *, #2236, .T. ) ;
#7883 = CARTESIAN_POINT ( 'NONE',  ( 0.8545932710616226391, 29.89685207198636618, -4.125402498422515052 ) ) ;
#7884 = EDGE_CURVE ( 'NONE', #9739, #15717, #11692, .T. ) ;
#7885 = ORIENTED_EDGE ( 'NONE', *, *, #14408, .T. ) ;
#7886 = CARTESIAN_POINT ( 'NONE',  ( -2.726577741920999998, 24.84881138680999868, -0.2402688989795999930 ) ) ;
#7888 = CARTESIAN_POINT ( 'NONE',  ( -0.4887088349126519349, 23.97504838153446016, 2.138075895062909293 ) ) ;
#7887 = DIRECTION ( 'NONE',  ( 0.000000000000000000, 1.000000000000000000, 0.000000000000000000 ) ) ;
#7889 = DIRECTION ( 'NONE',  ( 0.000000000000000000, 1.000000000000000000, 0.000000000000000000 ) ) ;
#7890 = VERTEX_POINT ( 'NONE', #16887 ) ;
#7891 = CARTESIAN_POINT ( 'NONE',  ( 17.29838745430000202, 0.2858153280860000200, 11.08860699072000067 ) ) ;
#7892 = CARTESIAN_POINT ( 'NONE',  ( -6.147641260848404343, 15.91672861095154801, 1.080128206638671928 ) ) ;
#7893 = EDGE_CURVE ( 'NONE', #14317, #3183, #6826, .T. ) ;
#7894 = CARTESIAN_POINT ( 'NONE',  ( -1.475897234648523293, 26.50000000000000711, 1.986511584949574249 ) ) ;
#7895 = EDGE_LOOP ( 'NONE', ( #12462, #5780, #11445 ) ) ;
#7896 = ORIENTED_EDGE ( 'NONE', *, *, #3908, .F. ) ;
#7897 = DIRECTION ( 'NONE',  ( -1.000000000000000000, 0.000000000000000000, 0.000000000000000000 ) ) ;
#7898 = CARTESIAN_POINT ( 'NONE',  ( -12.30419030543999881, 4.907441476050999896, -14.08182655546000106 ) ) ;
#7899 = CARTESIAN_POINT ( 'NONE',  ( 0.1910135035480641785, 6.779320233362403414, -1.743921721967714777 ) ) ;
#7900 = DIRECTION ( 'NONE',  ( 1.000000000000000000, 0.000000000000000000, 0.000000000000000000 ) ) ;
#7901 = ORIENTED_EDGE ( 'NONE', *, *, #4236, .F. ) ;
#7902 = CARTESIAN_POINT ( 'NONE',  ( -22.93116850624000236, 0.8725158193158999431, 10.19236064345000159 ) ) ;
#7903 = CARTESIAN_POINT ( 'NONE',  ( -23.86847083084828114, 7.985699633921027107, 11.16836250006974396 ) ) ;
#7904 = CARTESIAN_POINT ( 'NONE',  ( 6.214497071604325740, 13.81304699664710078, 1.115864161584470882 ) ) ;
#7905 = CARTESIAN_POINT ( 'NONE',  ( 15.66809006278837835, -8.888817418492333644, 5.302822816444082932 ) ) ;
#7906 = DIRECTION ( 'NONE',  ( 0.000000000000000000, 0.000000000000000000, -1.000000000000000000 ) ) ;
#7907 = CARTESIAN_POINT ( 'NONE',  ( -2.040625142429000505, 30.82237883270000012, 0.5584987965637999707 ) ) ;
#7908 = EDGE_CURVE ( 'NONE', #22927, #11959, #20367, .T. ) ;
#7909 = VECTOR ( 'NONE', #2000, 1000.000000000000000 ) ;
#7910 = B_SPLINE_CURVE_WITH_KNOTS ( 'NONE', 3,
 ( #19764, #12491, #23847, #3174, #1469, #8864, #5224, #17941 ),
 .UNSPECIFIED., .F., .F.,
 ( 4, 2, 2, 4 ),
 ( 0.000000000000000000, 0.2499999999999998890, 0.4999999999999997780, 1.000000000000000000 ),
 .UNSPECIFIED. ) ;
#7911 = CARTESIAN_POINT ( 'NONE',  ( -19.22500490859999900, -8.822855456895000614, 5.347747867906999630 ) ) ;
#7912 = CARTESIAN_POINT ( 'NONE',  ( 0.2000898907656600834, 29.61553224063326795, 2.150689853480966196 ) ) ;
#7913 = EDGE_LOOP ( 'NONE', ( #9057, #5565, #7401, #10798, #18391 ) ) ;
#7914 = CARTESIAN_POINT ( 'NONE',  ( -0.2530461047814999698, 25.00341469540000006, -2.171193274693999697 ) ) ;
#7915 = AXIS2_PLACEMENT_3D ( 'NONE', #12490, #18060, #3050 ) ;
#7916 = CARTESIAN_POINT ( 'NONE',  ( 7.446152422707000618, 28.20096189432300093, 6.000000000000000000 ) ) ;
#7917 = ORIENTED_EDGE ( 'NONE', *, *, #1582, .T. ) ;
#7918 = CARTESIAN_POINT ( 'NONE',  ( -2.251894740644691417, 24.64810525581627587, -0.1522571951427112991 ) ) ;
#7919 = CARTESIAN_POINT ( 'NONE',  ( -3.664365581929996285, 14.66068806201998420, 4.926677156548996628 ) ) ;
#7920 = CARTESIAN_POINT ( 'NONE',  ( 18.07245833333331930, -5.613829312641806624, 7.305091642245316486 ) ) ;
#7921 = EDGE_CURVE ( 'NONE', #3685, #20095, #2237, .T. ) ;
#7922 = CARTESIAN_POINT ( 'NONE',  ( 18.57487658530999752, 1.133029877492999882, 10.21722326572000128 ) ) ;
#7923 = EDGE_CURVE ( 'NONE', #20918, #10557, #10986, .T. ) ;
#7924 = ORIENTED_EDGE ( 'NONE', *, *, #12530, .T. ) ;
#7925 = CARTESIAN_POINT ( 'NONE',  ( -5.985231639314995356, 16.12312885759999403, -0.9718497405647000820 ) ) ;
#7926 = CARTESIAN_POINT ( 'NONE',  ( 24.00034722001000276, 7.216970193686000457, 11.92259671342000082 ) ) ;
#7927 = ORIENTED_EDGE ( 'NONE', *, *, #7717, .F. ) ;
#7928 = CARTESIAN_POINT ( 'NONE',  ( 0.000000000000000000, 20.10000000000000142, 0.000000000000000000 ) ) ;
#7929 = LINE ( 'NONE', #11807, #1630 ) ;
#7930 = CARTESIAN_POINT ( 'NONE',  ( 4.158710262565003646, 12.39730402461001013, 2.286416024636003019 ) ) ;
#7931 = AXIS2_PLACEMENT_3D ( 'NONE', #21829, #15994, #12626 ) ;
#7932 = CARTESIAN_POINT ( 'NONE',  ( 4.000000000000000000, 26.20000000000000284, 2.309401076759000304 ) ) ;
#7933 = CARTESIAN_POINT ( 'NONE',  ( 18.05736718707166588, -1.162665227242019039, -10.34590908488389438 ) ) ;
#7934 = CARTESIAN_POINT ( 'NONE',  ( 12.00000000000000000, 0.5465009267866380860, -9.295035738989342988 ) ) ;
#7935 = CARTESIAN_POINT ( 'NONE',  ( 0.000000000000000000, 20.10000000000000142, 0.000000000000000000 ) ) ;
#7937 = EDGE_CURVE ( 'NONE', #3633, #11154, #22815, .T. ) ;
#7936 = CARTESIAN_POINT ( 'NONE',  ( -3.985645024478002174, 15.21034615980000737, -4.691483454359003602 ) ) ;
#7938 = ADVANCED_FACE ( 'NONE', ( #4302 ), #9916, .F. ) ;
#7939 = DIRECTION ( 'NONE',  ( -1.000000000000000000, 0.000000000000000000, 0.000000000000000000 ) ) ;
#7940 = CARTESIAN_POINT ( 'NONE',  ( 5.155702020191999857, 13.97328941143999970, -4.008166040501000893 ) ) ;
#7941 = DIRECTION ( 'NONE',  ( 0.000000000000000000, 1.000000000000000000, 0.000000000000000000 ) ) ;
#7942 = CARTESIAN_POINT ( 'NONE',  ( 0.09195743698950356593, 30.40914314436703592, 2.158523876181588808 ) ) ;
#7943 = VERTEX_POINT ( 'NONE', #14944 ) ;
#7944 = CARTESIAN_POINT ( 'NONE',  ( 22.10697221064000217, -9.368869399783999796, 3.007899085511000159 ) ) ;
#7945 = CARTESIAN_POINT ( 'NONE',  ( -0.5803961911334408752, 12.81517387975837785, -6.641171340469228745 ) ) ;
#7946 = CARTESIAN_POINT ( 'NONE',  ( -23.53040576725368282, -6.468648380949139742, -6.731035015224344775 ) ) ;
#7947 = CARTESIAN_POINT ( 'NONE',  ( -22.75960804221382716, -9.535639810683969486, -4.553883601656974811 ) ) ;
#7948 = CARTESIAN_POINT ( 'NONE',  ( -2.406140597653999791, 26.04946440326000001, 0.5279260092677999783 ) ) ;
#7949 = AXIS2_PLACEMENT_3D ( 'NONE', #6050, #2424, #17078 ) ;
#7950 = FACE_OUTER_BOUND ( 'NONE', #17124, .T. ) ;
#7951 = ORIENTED_EDGE ( 'NONE', *, *, #12545, .F. ) ;
#7952 = CARTESIAN_POINT ( 'NONE',  ( -19.16365649254885994, -9.894903494359850171, -3.434324854208239852 ) ) ;
#7953 = CARTESIAN_POINT ( 'NONE',  ( 0.5271288625574210851, 26.26111511314614688, 2.095841999210956264 ) ) ;
#7954 = CARTESIAN_POINT ( 'NONE',  ( 0.1848998096957392423, 27.84077103474808723, 2.192915077246018196 ) ) ;
#7955 = CARTESIAN_POINT ( 'NONE',  ( 11.50000000000000000, 0.000000000000000000, -7.000000000000000000 ) ) ;
#7956 = ORIENTED_EDGE ( 'NONE', *, *, #4864, .T. ) ;
#7957 = CARTESIAN_POINT ( 'NONE',  ( -15.91276253787999728, 9.079634562165001199, 0.000000000000000000 ) ) ;
#7958 = CARTESIAN_POINT ( 'NONE',  ( 13.66537674931000090, -8.233391669162999804, 6.770876163316000174 ) ) ;
#7959 = CONICAL_SURFACE ( 'NONE', #2145, 4.699999872533999756, 0.7853981633972997312 ) ;
#7960 = CARTESIAN_POINT ( 'NONE',  ( -14.95375200203000077, 10.81627527975999925, -3.353864774601000409 ) ) ;
#7961 = DIRECTION ( 'NONE',  ( 1.000000000000000000, 0.000000000000000000, 0.000000000000000000 ) ) ;
#7962 = CARTESIAN_POINT ( 'NONE',  ( 14.65046080086000124, 8.467099989590000320, -7.526153856646999429 ) ) ;
#7963 = CARTESIAN_POINT ( 'NONE',  ( -7.500000000000000000, 24.99999999999999645, 1.000000000000000000 ) ) ;
#7964 = AXIS2_PLACEMENT_3D ( 'NONE', #13243, #20753, #18465 ) ;
#7965 = DIRECTION ( 'NONE',  ( 6.904857654351749962E-20, 1.420096922000000058E-10, -1.000000000000000000 ) ) ;
#7966 = CARTESIAN_POINT ( 'NONE',  ( 23.14589779687000259, -1.191954907644999784, 10.21085767065999939 ) ) ;
#7967 = LINE ( 'NONE', #11609, #20476 ) ;
#7968 = ORIENTED_EDGE ( 'NONE', *, *, #7178, .F. ) ;
#7969 = CARTESIAN_POINT ( 'NONE',  ( 22.66677564524290744, 35.31760589360604996, 6.000000000000000000 ) ) ;
#7970 = CARTESIAN_POINT ( 'NONE',  ( 2.844001364980000002, 26.87750240009999914, -0.3933730402103999824 ) ) ;
#7971 = CARTESIAN_POINT ( 'NONE',  ( -4.707944767739004277, 12.53013094992000021, 0.4102711938274001824 ) ) ;
#7972 = CARTESIAN_POINT ( 'NONE',  ( 61.60588651278290939, 37.01856778792605240, -1.000000000000000000 ) ) ;
#7973 = CARTESIAN_POINT ( 'NONE',  ( -21.43440823118999816, -8.843504048032999165, 6.691333516387000913 ) ) ;
#7974 = EDGE_LOOP ( 'NONE', ( #7436, #10656, #21169, #3242 ) ) ;
#7975 = FACE_OUTER_BOUND ( 'NONE', #9557, .T. ) ;
#7976 = ORIENTED_EDGE ( 'NONE', *, *, #1724, .F. ) ;
#7977 = CYLINDRICAL_SURFACE ( 'NONE', #9147, 2.500000000000000000 ) ;
#7978 = LINE ( 'NONE', #17177, #7370 ) ;
#7979 = DIRECTION ( 'NONE',  ( -1.000000000000000000, 0.000000000000000000, 0.000000000000000000 ) ) ;
#7980 = TOROIDAL_SURFACE ( 'NONE', #16098, 2.100000000000000089, 0.1000000000000000056 ) ;
#7981 = AXIS2_PLACEMENT_3D ( 'NONE', #17927, #23112, #2912 ) ;
#7982 = CARTESIAN_POINT ( 'NONE',  ( -0.1076860494153716596, 6.777623460670147537, 1.750377179531549254 ) ) ;
#7983 = CARTESIAN_POINT ( 'NONE',  ( 16.51725174930999884, 10.44001970777000032, -2.498676648948999990 ) ) ;
#7984 = CARTESIAN_POINT ( 'NONE',  ( -14.98621963600000129, -7.639996621784999498, -6.839520901588999280 ) ) ;
#7985 = CARTESIAN_POINT ( 'NONE',  ( 13.58606375731000071, 0.1873974521201000054, -9.128548663592997769 ) ) ;
#7986 = CARTESIAN_POINT ( 'NONE',  ( -14.45529023502158417, -2.584742736866077806, 12.49997119546092428 ) ) ;
#7987 = VERTEX_POINT ( 'NONE', #17135 ) ;
#7988 = CARTESIAN_POINT ( 'NONE',  ( 2.711127088422999876, 30.87230859155000218, -0.2628573326712999592 ) ) ;
#7989 = CARTESIAN_POINT ( 'NONE',  ( 2.446868772696999983, 24.51702865104000040, 1.178890382843999829 ) ) ;
#7990 = CARTESIAN_POINT ( 'NONE',  ( 14.24134250575724536, -7.125643292243364790, -7.467448625278665375 ) ) ;
#7991 = CARTESIAN_POINT ( 'NONE',  ( 4.524261242948997896, 14.78625385561000982, -4.165603776964002414 ) ) ;
#7992 = CARTESIAN_POINT ( 'NONE',  ( 2.000000000000000000, 18.89999999999999858, 0.000000000000000000 ) ) ;
#7993 = CARTESIAN_POINT ( 'NONE',  ( -0.8857055135539000368, 28.33000425264999933, 2.448665480424999874 ) ) ;
#7994 = CARTESIAN_POINT ( 'NONE',  ( 11.36448692216853829, -2.758025466591909058, 12.49997558795521080 ) ) ;
#7995 = CARTESIAN_POINT ( 'NONE',  ( 17.79316524073560046, -3.565549168114876100, -9.974336391710325600 ) ) ;
#7996 = AXIS2_PLACEMENT_3D ( 'NONE', #11210, #5744, #16873 ) ;
#7997 = CARTESIAN_POINT ( 'NONE',  ( -9.000000000000000000, 18.50000000000000000, -2.000000000000000000 ) ) ;
#7998 = DIRECTION ( 'NONE',  ( -1.000000000000000000, 0.000000000000000000, 0.000000000000000000 ) ) ;
#7999 = EDGE_CURVE ( 'NONE', #4782, #21708, #18781, .T. ) ;
#8000 = DIRECTION ( 'NONE',  ( 0.000000000000000000, 0.000000000000000000, -1.000000000000000000 ) ) ;
#8001 = ORIENTED_EDGE ( 'NONE', *, *, #2403, .F. ) ;
#8002 = DIRECTION ( 'NONE',  ( 8.130136936064000824E-11, 0.000000000000000000, 1.000000000000000000 ) ) ;
#8003 = EDGE_LOOP ( 'NONE', ( #23123, #6927, #17605, #16332, #21601, #7772 ) ) ;
#8004 = CARTESIAN_POINT ( 'NONE',  ( 1.988422905474999780, 25.96353585921000118, 1.881031091488000184 ) ) ;
#8006 = DIRECTION ( 'NONE',  ( 1.000000000000000000, 0.000000000000000000, 0.000000000000000000 ) ) ;
#8005 = CARTESIAN_POINT ( 'NONE',  ( -2.443031855719502321, 11.73523197788490613, 4.158142541589644026 ) ) ;
#8007 = CARTESIAN_POINT ( 'NONE',  ( 3.099999776787000005, 15.00000022320933013, 5.570936504208000122E-07 ) ) ;
#8008 = AXIS2_PLACEMENT_3D ( 'NONE', #16817, #7619, #2167 ) ;
#8009 = CARTESIAN_POINT ( 'NONE',  ( 13.86982039523999966, -6.786930149467000462, 8.654887823694998872 ) ) ;
#8010 = CARTESIAN_POINT ( 'NONE',  ( -20.68792035241834171, 2.624964421005299808, 8.884893743000107591 ) ) ;
#8011 = CARTESIAN_POINT ( 'NONE',  ( -0.8020744510286262896, 26.50000000000000355, 2.262007200476410684 ) ) ;
#8012 = EDGE_CURVE ( 'NONE', #19991, #11598, #19202, .T. ) ;
#8013 = EDGE_LOOP ( 'NONE', ( #14873, #2175, #11610, #18404, #4697, #18295, #6940, #10054, #6830 ) ) ;
#8014 = ORIENTED_EDGE ( 'NONE', *, *, #18883, .F. ) ;
#8015 = CIRCLE ( 'NONE', #21573, 2.270871215252209030 ) ;
#8016 = CARTESIAN_POINT ( 'NONE',  ( -13.99999999999999822, 1.175534018597250263, -9.359874577866060363 ) ) ;
#8017 = FACE_OUTER_BOUND ( 'NONE', #18150, .T. ) ;
#8018 = CARTESIAN_POINT ( 'NONE',  ( -14.47826289458183524, -9.918718668888027779, -7.820280362116103667 ) ) ;
#8019 = ORIENTED_EDGE ( 'NONE', *, *, #16502, .F. ) ;
#8020 = CARTESIAN_POINT ( 'NONE',  ( -21.48771292778999964, 7.737897503461000248, -5.795162599746999987 ) ) ;
#8021 = CARTESIAN_POINT ( 'NONE',  ( 2.327192509895193329, 28.00639765414753057, -3.274853329251975698 ) ) ;
#8022 = DIRECTION ( 'NONE',  ( 0.000000000000000000, -1.000000000000000000, 0.000000000000000000 ) ) ;
#8023 = CARTESIAN_POINT ( 'NONE',  ( 15.36333275736410009, 0.2825445565885951749, 10.35592818220791145 ) ) ;
#8024 = CARTESIAN_POINT ( 'NONE',  ( -18.16404412701000126, -2.121094635088999869, 10.90079736569000168 ) ) ;
#8025 = DIRECTION ( 'NONE',  ( 1.000000000000000000, 0.000000000000000000, 0.000000000000000000 ) ) ;
#8026 = CARTESIAN_POINT ( 'NONE',  ( -20.27843488810067285, 10.02134192589039330, 3.140444712618212009 ) ) ;
#8027 = AXIS2_PLACEMENT_3D ( 'NONE', #948, #1072, #6279 ) ;
#8028 = CARTESIAN_POINT ( 'NONE',  ( -16.44889015301999891, 10.17473773424000072, -3.711315847300999948 ) ) ;
#8029 = EDGE_CURVE ( 'NONE', #4988, #11075, #7590, .T. ) ;
#8030 = CARTESIAN_POINT ( 'NONE',  ( -0.01426998130716234520, 29.60301338715854058, 2.159908921319442232 ) ) ;
#8031 = ORIENTED_EDGE ( 'NONE', *, *, #2163, .T. ) ;
#8032 = CARTESIAN_POINT ( 'NONE',  ( 0.6119580278259999506, 25.45552357783000019, 2.267762994067999749 ) ) ;
#8033 = CARTESIAN_POINT ( 'NONE',  ( -18.39874231378647096, 9.042411196046327149, 5.258422072222084687 ) ) ;
#8034 = APPLICATION_CONTEXT ( 'automotive_design' ) ;
#8035 = ORIENTED_EDGE ( 'NONE', *, *, #21197, .F. ) ;
#8036 = CARTESIAN_POINT ( 'NONE',  ( 0.4476285504030235729, 30.41139891206333346, -2.497755735888799400 ) ) ;
#8037 = DIRECTION ( 'NONE',  ( 0.000000000000000000, -1.000000000000000000, 0.000000000000000000 ) ) ;
#8038 = CARTESIAN_POINT ( 'NONE',  ( 1.699999999999999956, 9.063112730255063809, -0.9835110234548531949 ) ) ;
#8039 = ADVANCED_FACE ( 'NONE', ( #897, #23420 ), #19445, .T. ) ;
#8040 = CARTESIAN_POINT ( 'NONE',  ( 15.58687642131000040, -1.771707419409999984, -9.528874100789000323 ) ) ;
#8041 = B_SPLINE_CURVE_WITH_KNOTS ( 'NONE', 3,
 ( #286, #17369, #9504, #7687, #22685, #11683, #15177, #2230, #16878, #4054, #15538, #22805 ),
 .UNSPECIFIED., .F., .F.,
 ( 4, 1, 1, 1, 1, 2, 2, 4 ),
 ( 0.000000000000000000, 0.2499999999999964473, 0.3749999999999947820, 0.4374999999999936717, 0.4687499999999933387, 0.4843749999999933942, 0.4999999999999934497, 1.000000000000000000 ),
 .UNSPECIFIED. ) ;
#8042 = ORIENTED_EDGE ( 'NONE', *, *, #20223, .T. ) ;
#8043 = CARTESIAN_POINT ( 'NONE',  ( -7.500000000000000000, 24.99999999999999645, 1.000000000000000000 ) ) ;
#8044 = VECTOR ( 'NONE', #12837, 1000.000000000000000 ) ;
#8045 = DIRECTION ( 'NONE',  ( -0.1556330747009919968, -0.9878149351265710365, 5.988626934220810756E-08 ) ) ;
#8046 = CARTESIAN_POINT ( 'NONE',  ( 23.99478584078000054, 6.383504859148000143, 12.40379814867000086 ) ) ;
#8047 = PRODUCT_DEFINITION_SHAPE ( 'NONE', 'NONE',  #5757 ) ;
#8048 = VERTEX_POINT ( 'NONE', #8661 ) ;
#8049 = CARTESIAN_POINT ( 'NONE',  ( -1.799315205405667806, 24.70347107637078565, 1.274838228386613093 ) ) ;
#8050 = DIRECTION ( 'NONE',  ( 0.000000000000000000, 1.000000000000000000, 0.000000000000000000 ) ) ;
#8051 = CARTESIAN_POINT ( 'NONE',  ( 24.11771641471887406, 4.428067703116305154, 9.651354340895641926 ) ) ;
#8052 = FACE_OUTER_BOUND ( 'NONE', #6392, .T. ) ;
#8053 = CARTESIAN_POINT ( 'NONE',  ( 18.21437946870691960, 4.352035995711678318, -9.479931473404731079 ) ) ;
#8054 = EDGE_CURVE ( 'NONE', #9910, #6464, #10712, .T. ) ;
#8055 = CONICAL_SURFACE ( 'NONE', #3804, 12.68487026514999982, 0.6105562205522639951 ) ;
#8056 = DIRECTION ( 'NONE',  ( 0.000000000000000000, -1.000000000000000000, 0.000000000000000000 ) ) ;
#8057 = CARTESIAN_POINT ( 'NONE',  ( 19.45270603379666241, 8.931744951680411049, -2.400470103937684563 ) ) ;
#8058 = CARTESIAN_POINT ( 'NONE',  ( -4.464533626733999228, 14.94938198047000455, -3.893093625067998165 ) ) ;
#8059 = DIRECTION ( 'NONE',  ( 1.000000000000000000, 0.000000000000000000, 0.000000000000000000 ) ) ;
#8060 = STYLED_ITEM ( 'NONE', ( #14457 ), #16570 ) ;
#8061 = CARTESIAN_POINT ( 'NONE',  ( 5.415137083822752828, 14.57951453618345639, 2.868756701730457603 ) ) ;
#8062 = CARTESIAN_POINT ( 'NONE',  ( 1.500000000000000000, 7.100000000000000533, 0.000000000000000000 ) ) ;
#8063 = ADVANCED_FACE ( 'NONE', ( #17381 ), #4422, .F. ) ;
#8064 = CARTESIAN_POINT ( 'NONE',  ( -0.02785460051843529836, 30.40211518515314282, 2.159877924567529028 ) ) ;
#8065 = ORIENTED_EDGE ( 'NONE', *, *, #2225, .T. ) ;
#8066 = EDGE_CURVE ( 'NONE', #5788, #15508, #16163, .T. ) ;
#8067 = CARTESIAN_POINT ( 'NONE',  ( -16.82566243917332471, -4.584591771195801968, 7.954082539197118606 ) ) ;
#8068 = CARTESIAN_POINT ( 'NONE',  ( 24.58366860467999970, -9.697657171452000568, 6.209474635623999816 ) ) ;
#8069 = CARTESIAN_POINT ( 'NONE',  ( -3.174784089423522193, 13.14313549967478778, -5.966242404707048586 ) ) ;
#8070 = DIRECTION ( 'NONE',  ( 0.000000000000000000, 0.000000000000000000, -1.000000000000000000 ) ) ;
#8071 = CIRCLE ( 'NONE', #10411, 2.729128784747790970 ) ;
#8072 = CARTESIAN_POINT ( 'NONE',  ( -19.94808866505225708, 7.612438129746494475, 7.224177472218721974 ) ) ;
#8073 = CARTESIAN_POINT ( 'NONE',  ( -3.644450799678000230, 14.33206891749000000, -4.922778709793999674 ) ) ;
#8074 = CARTESIAN_POINT ( 'NONE',  ( 0.000000000000000000, 24.49999999999999645, 0.000000000000000000 ) ) ;
#8075 = VERTEX_POINT ( 'NONE', #9254 ) ;
#8076 = AXIS2_PLACEMENT_3D ( 'NONE', #20488, #9461, #16835 ) ;
#8077 = CARTESIAN_POINT ( 'NONE',  ( -17.32151483542483561, -9.473612476238717051, -4.362928530524290416 ) ) ;
#8078 = ADVANCED_FACE ( 'NONE', ( #20277 ), #1458, .F. ) ;
#8079 = CARTESIAN_POINT ( 'NONE',  ( 4.000000000000000000, 24.80000000000000426, 2.309401076759000304 ) ) ;
#8080 = ADVANCED_FACE ( 'NONE', ( #19160 ), #13780, .T. ) ;
#8081 = CONICAL_SURFACE ( 'NONE', #21627, 2.250000000000000000, 0.7853981633972997312 ) ;
#8082 = CARTESIAN_POINT ( 'NONE',  ( -0.1005214697688198294, 28.23526083320289715, -2.196413288871530423 ) ) ;
#8083 = DIRECTION ( 'NONE',  ( 0.000000000000000000, 1.000000000000000000, 0.000000000000000000 ) ) ;
#8084 = VERTEX_POINT ( 'NONE', #2571 ) ;
#8085 = CARTESIAN_POINT ( 'NONE',  ( 17.71428936713000013, 9.125865291226999076, 0.000000000000000000 ) ) ;
#8086 = VECTOR ( 'NONE', #9789, 1000.000000000000000 ) ;
#8087 = CARTESIAN_POINT ( 'NONE',  ( 14.54287674931000041, 7.516034287427999949, -7.591774476630000379 ) ) ;
#8088 = CARTESIAN_POINT ( 'NONE',  ( -22.61365783827999820, -1.438403498588999962, -11.09373300380999972 ) ) ;
#8089 = CARTESIAN_POINT ( 'NONE',  ( -15.36001269797000113, -1.548705033035999934, -11.22934907313000075 ) ) ;
#8090 = PLANE ( 'NONE',  #3084 ) ;
#8091 = CARTESIAN_POINT ( 'NONE',  ( 19.05244494525999954, 10.34262564730999934, 0.7747601940386998898 ) ) ;
#8092 = CARTESIAN_POINT ( 'NONE',  ( -4.000000000000000000, 26.50000000000000355, 0.000000000000000000 ) ) ;
#8093 = CARTESIAN_POINT ( 'NONE',  ( -24.50000000000000000, 7.216878364870000340, -12.50000000000000000 ) ) ;
#8094 = CARTESIAN_POINT ( 'NONE',  ( 21.19835767317000119, 3.471603973022999945, 9.619727525801000212 ) ) ;
#8095 = VECTOR ( 'NONE', #19501, 1000.000000000000114 ) ;
#8096 = CARTESIAN_POINT ( 'NONE',  ( -5.730762473771000565, 26.50000000000000000, 1.577381738259000077 ) ) ;
#8097 = VERTEX_POINT ( 'NONE', #2826 ) ;
#8098 = CARTESIAN_POINT ( 'NONE',  ( -4.000000000000000000, 24.80000000000000426, 2.309401076759000304 ) ) ;
#8099 = CARTESIAN_POINT ( 'NONE',  ( 2.747163055864000114, 26.09750240010000155, -0.8328668639933000106 ) ) ;
#8100 = AXIS2_PLACEMENT_3D ( 'NONE', #21800, #4735, #5215 ) ;
#8101 = CARTESIAN_POINT ( 'NONE',  ( 4.204466630777001335, 12.26413482981000236, 2.286142766050001107 ) ) ;
#8102 = LINE ( 'NONE', #15102, #15795 ) ;
#8103 = CARTESIAN_POINT ( 'NONE',  ( -21.45487118009000227, -3.743657570342999730, 10.43929364024000073 ) ) ;
#8104 = VERTEX_POINT ( 'NONE', #14077 ) ;
#8105 = FACE_OUTER_BOUND ( 'NONE', #19148, .T. ) ;
#8106 = AXIS2_PLACEMENT_3D ( 'NONE', #14265, #23700, #3602 ) ;
#8107 = ORIENTED_EDGE ( 'NONE', *, *, #1724, .T. ) ;
#8108 = DIRECTION ( 'NONE',  ( -1.000000000000000000, 0.000000000000000000, 0.000000000000000000 ) ) ;
#8109 = DIRECTION ( 'NONE',  ( 2.317847042770929243E-07, 0.9999999999999731326, 0.000000000000000000 ) ) ;
#8110 = EDGE_CURVE ( 'NONE', #3493, #479, #7496, .T. ) ;
#8111 = DIRECTION ( 'NONE',  ( 1.000000000000000000, 0.000000000000000000, 0.000000000000000000 ) ) ;
#8112 = CARTESIAN_POINT ( 'NONE',  ( -1.077644597311803620, 6.862813149403997670, 1.379208851604670993 ) ) ;
#8113 = CARTESIAN_POINT ( 'NONE',  ( -14.25547362505000137, 7.466449067002999485, 11.77856001874999947 ) ) ;
#8114 = AXIS2_PLACEMENT_3D ( 'NONE', #5886, #9882, #11592 ) ;
#8115 = CARTESIAN_POINT ( 'NONE',  ( -13.76743754818000021, -2.422432655768999687, 9.928996171009998761 ) ) ;
#8116 = CIRCLE ( 'NONE', #3859, 4.000000000000000000 ) ;
#8117 = CARTESIAN_POINT ( 'NONE',  ( 13.03762625731000036, -8.686210121801000383, 2.766264305181999728 ) ) ;
#8118 = DIRECTION ( 'NONE',  ( 0.000000000000000000, 0.000000000000000000, -1.000000000000000000 ) ) ;
#8119 = EDGE_LOOP ( 'NONE', ( #23908, #5513, #21313, #7322, #2698 ) ) ;
#8120 = CARTESIAN_POINT ( 'NONE',  ( 18.99957840953792854, -6.685677144414598594, 8.077138694963919008 ) ) ;
#8121 = CARTESIAN_POINT ( 'NONE',  ( -4.900699999999999612, 1.284663064832999817E-14, 0.000000000000000000 ) ) ;
#8122 = CARTESIAN_POINT ( 'NONE',  ( -1.399447169867999996, 23.70324008177000152, 1.869294607855000123 ) ) ;
#8123 = CARTESIAN_POINT ( 'NONE',  ( 13.54165762163843212, 0.5435700620289271034, 10.30418047178718943 ) ) ;
#8124 = VERTEX_POINT ( 'NONE', #8154 ) ;
#8125 = CARTESIAN_POINT ( 'NONE',  ( 4.270538739245997029, 13.49097647299000791, -4.885090785149001746 ) ) ;
#8126 = LINE ( 'NONE', #7757, #2276 ) ;
#8127 = LINE ( 'NONE', #6415, #11935 ) ;
#8128 = CARTESIAN_POINT ( 'NONE',  ( 11.78693030655488982, -4.312506568626711889, 12.49999836761128869 ) ) ;
#8129 = DIRECTION ( 'NONE',  ( 0.000000000000000000, 1.000000000000000000, 0.000000000000000000 ) ) ;
#8130 = DIRECTION ( 'NONE',  ( 0.000000000000000000, 1.000000000000000000, 0.000000000000000000 ) ) ;
#8131 = CARTESIAN_POINT ( 'NONE',  ( -21.43624577250665197, 2.413793474093852698, -8.981321659912415711 ) ) ;
#8132 = CARTESIAN_POINT ( 'NONE',  ( -0.3272492347489394104, 29.65086340285666466, -2.499999999999999112 ) ) ;
#8133 = ORIENTED_EDGE ( 'NONE', *, *, #12006, .T. ) ;
#8134 = DIRECTION ( 'NONE',  ( -1.000000000000000000, 0.000000000000000000, 0.000000000000000000 ) ) ;
#8135 = ORIENTED_EDGE ( 'NONE', *, *, #7439, .F. ) ;
#8136 = CARTESIAN_POINT ( 'NONE',  ( 0.000000000000000000, 21.95000012746600149, 0.000000000000000000 ) ) ;
#8138 = CARTESIAN_POINT ( 'NONE',  ( 1.440866150671271440, 24.31242210092122491, -1.654208956319656032 ) ) ;
#8137 = DIRECTION ( 'NONE',  ( -6.134662446597347369E-06, -0.9780939470516456513, 0.2081639514980881955 ) ) ;
#8139 = DIRECTION ( 'NONE',  ( 0.000000000000000000, 1.000000000000000000, 0.000000000000000000 ) ) ;
#8140 = CARTESIAN_POINT ( 'NONE',  ( -6.331662004670999266, 15.27947543293999821, -1.623597805356998602 ) ) ;
#8141 = CARTESIAN_POINT ( 'NONE',  ( -0.9779981048622099493, 26.50000000000000711, 2.217847022944143376 ) ) ;
#8142 = ORIENTED_EDGE ( 'NONE', *, *, #10113, .T. ) ;
#8143 = ORIENTED_EDGE ( 'NONE', *, *, #1275, .F. ) ;
#8144 = CARTESIAN_POINT ( 'NONE',  ( -14.00000000000000000, 1.110052840749007119, -9.371533619972057139 ) ) ;
#8145 = CARTESIAN_POINT ( 'NONE',  ( 2.000000000000000000, 30.00000000000000000, -3.464101615137999968 ) ) ;
#8146 = CARTESIAN_POINT ( 'NONE',  ( -24.36724102300192740, -9.545677019768170624, -8.466242377946848308 ) ) ;
#8147 = EDGE_CURVE ( 'NONE', #15650, #14474, #4644, .T. ) ;
#8148 = ORIENTED_EDGE ( 'NONE', *, *, #11874, .T. ) ;
#8149 = CARTESIAN_POINT ( 'NONE',  ( -19.08857862928000060, 1.783951728274999926, 9.434913288203000903 ) ) ;
#8150 = DIRECTION ( 'NONE',  ( 1.000000000000000000, 0.000000000000000000, 0.000000000000000000 ) ) ;
#8151 = CARTESIAN_POINT ( 'NONE',  ( 6.233508746500216802, 13.72128517286145666, 1.472007961487105554 ) ) ;
#8152 = CARTESIAN_POINT ( 'NONE',  ( 15.78996759782221737, -10.28928894160047314, 1.185823107492882666 ) ) ;
#8153 = CARTESIAN_POINT ( 'NONE',  ( -16.71873760674999687, 9.784722624912999933, 5.167966991771000274 ) ) ;
#8154 = CARTESIAN_POINT ( 'NONE',  ( 0.000000000000000000, 20.00000000000000000, -4.649999999999999467 ) ) ;
#8155 = CARTESIAN_POINT ( 'NONE',  ( -20.43284564258691560, 10.22652009526272110, -2.407089174038743451 ) ) ;
#8156 = CARTESIAN_POINT ( 'NONE',  ( -13.10414243475000085, 9.447148007457000674, -4.942668164112999918 ) ) ;
#8157 = CARTESIAN_POINT ( 'NONE',  ( -1.918585267525981797, 29.34217026962017982, -1.008785855482386973 ) ) ;
#8158 = EDGE_LOOP ( 'NONE', ( #15191, #18945, #11884, #2549, #22148, #5002 ) ) ;
#8159 = CARTESIAN_POINT ( 'NONE',  ( -2.122260425170999998, 24.47835486083999967, 1.006620808079000007 ) ) ;
#8160 = CARTESIAN_POINT ( 'NONE',  ( -15.85209501512817987, -10.37091023683542801, 0.7487072676850166086 ) ) ;
#8161 = CIRCLE ( 'NONE', #10490, 1.000000000000000000 ) ;
#8162 = ORIENTED_EDGE ( 'NONE', *, *, #1138, .F. ) ;
#8163 = CARTESIAN_POINT ( 'NONE',  ( 6.067719036437005720, 14.08021635583998155, -0.4562290550031999348 ) ) ;
#8164 = CARTESIAN_POINT ( 'NONE',  ( 0.000000000000000000, 7.000000000000000000, 0.000000000000000000 ) ) ;
#8165 = CARTESIAN_POINT ( 'NONE',  ( 3.050000000000000266, 18.50000000000000000, 0.000000000000000000 ) ) ;
#8166 = CARTESIAN_POINT ( 'NONE',  ( 11.52843892131000025, -9.307182416847998851, 0.9706197651944000748 ) ) ;
#8167 = ORIENTED_EDGE ( 'NONE', *, *, #14699, .F. ) ;
#8168 = DIRECTION ( 'NONE',  ( 1.000000000000000000, 0.000000000000000000, 0.000000000000000000 ) ) ;
#8169 = CARTESIAN_POINT ( 'NONE',  ( -0.6543697108982037269, 27.03333333333333499, -2.434931691670788823 ) ) ;
#8170 = DIRECTION ( 'NONE',  ( 0.000000000000000000, 1.000000000000000000, 0.000000000000000000 ) ) ;
#8171 = EDGE_CURVE ( 'NONE', #10966, #8048, #17723, .T. ) ;
#8172 = ORIENTED_EDGE ( 'NONE', *, *, #23537, .F. ) ;
#8173 = DIRECTION ( 'NONE',  ( -1.000000000000000000, 0.000000000000000000, 0.000000000000000000 ) ) ;
#8174 = DIRECTION ( 'NONE',  ( 0.000000000000000000, -1.000000000000000000, 0.000000000000000000 ) ) ;
#8175 = CARTESIAN_POINT ( 'NONE',  ( -23.19747332303477449, 9.265518480805006618, -0.8872243700272733902 ) ) ;
#8176 = DIRECTION ( 'NONE',  ( 0.000000000000000000, 0.000000000000000000, 1.000000000000000000 ) ) ;
#8177 = CARTESIAN_POINT ( 'NONE',  ( 18.32885411205448989, 7.626691132225033698, -7.100304570260450809 ) ) ;
#8178 = CARTESIAN_POINT ( 'NONE',  ( 12.00000000000000178, -5.850718947441217566, -7.765274011324477144 ) ) ;
#8179 = CARTESIAN_POINT ( 'NONE',  ( -14.49454883410026262, 11.27877807214811412, -5.464517788383438379 ) ) ;
#8180 = CARTESIAN_POINT ( 'NONE',  ( 23.94234578240000033, 6.585182621219000332, 9.182389591044998411 ) ) ;
#8181 = CARTESIAN_POINT ( 'NONE',  ( 0.000000000000000000, 20.00000000000000000, 0.000000000000000000 ) ) ;
#8182 = DIRECTION ( 'NONE',  ( 6.905631305162550971E-20, -1.420100391446999833E-10, 1.000000000000000000 ) ) ;
#8183 = CARTESIAN_POINT ( 'NONE',  ( 0.000000000000000000, 24.29999999999999716, 0.000000000000000000 ) ) ;
#8184 = EDGE_CURVE ( 'NONE', #259, #14234, #11906, .T. ) ;
#8185 = CARTESIAN_POINT ( 'NONE',  ( -2.159897835357240226, 30.20132937181709565, -0.03950432281413149282 ) ) ;
#8186 = ORIENTED_EDGE ( 'NONE', *, *, #19951, .T. ) ;
#8187 = CARTESIAN_POINT ( 'NONE',  ( 18.92682980101000112, -9.687490077531000665, 4.826695779770999728 ) ) ;
#8188 = CARTESIAN_POINT ( 'NONE',  ( 4.308859103450683570, 13.42278743254423468, -5.306801479098574248 ) ) ;
#8189 = CARTESIAN_POINT ( 'NONE',  ( -23.66575074361468012, -9.444067616000523913, -0.7617870456259082657 ) ) ;
#8190 = CARTESIAN_POINT ( 'NONE',  ( -20.05519416513632791, 9.717599291601674238, 3.967186786816359501 ) ) ;
#8191 = CARTESIAN_POINT ( 'NONE',  ( 4.906142749732728348, 14.36517199318403648, 3.820454354895810312 ) ) ;
#8192 = CARTESIAN_POINT ( 'NONE',  ( -6.173093822438193712, 26.49020434458659068, 1.113528899897020308 ) ) ;
#8193 = ORIENTED_EDGE ( 'NONE', *, *, #14930, .F. ) ;
#8194 = EDGE_CURVE ( 'NONE', #18434, #9620, #5204, .T. ) ;
#8195 = CARTESIAN_POINT ( 'NONE',  ( -18.49378679904955902, 9.238542528155839761, -4.896975808983531131 ) ) ;
#8196 = AXIS2_PLACEMENT_3D ( 'NONE', #1016, #14347, #17621 ) ;
#8197 = CARTESIAN_POINT ( 'NONE',  ( -12.50000000000000000, 10.59999999999999964, 0.000000000000000000 ) ) ;
#8198 = CARTESIAN_POINT ( 'NONE',  ( 1.977975842973895393, 28.08732715878234387, -0.9681838510627849281 ) ) ;
#8199 =( NAMED_UNIT ( * ) SI_UNIT ( $, .STERADIAN. ) SOLID_ANGLE_UNIT ( ) );
#8200 = CARTESIAN_POINT ( 'NONE',  ( -14.06668704121266877, 9.028294978683996774, 1.058664089371861072 ) ) ;
#8201 = ADVANCED_FACE ( 'NONE', ( #6571 ), #1794, .T. ) ;
#8202 = ORIENTED_EDGE ( 'NONE', *, *, #14605, .F. ) ;
#8203 = CARTESIAN_POINT ( 'NONE',  ( 4.000000000000001776, 29.97444252552741872, -0.7494995952805654227 ) ) ;
#8204 = CARTESIAN_POINT ( 'NONE',  ( 18.05287674931000197, 3.913226583351999910, -10.03953908883999979 ) ) ;
#8205 = CARTESIAN_POINT ( 'NONE',  ( -22.29248446835000053, 9.305055704266001371, -6.193688370995000803 ) ) ;
#8206 = CARTESIAN_POINT ( 'NONE',  ( -15.49211357277000012, 9.807665638945000097, -3.040989941390000340 ) ) ;
#8207 = CARTESIAN_POINT ( 'NONE',  ( 21.96499999999999986, -9.234946903777000671, 0.000000000000000000 ) ) ;
#8208 = CARTESIAN_POINT ( 'NONE',  ( 14.17744494526000132, -4.616554532313999815, 9.135639917857000469 ) ) ;
#8209 = CARTESIAN_POINT ( 'NONE',  ( 2.100000000000000089, 19.00000000000000000, 0.000000000000000000 ) ) ;
#8210 = DIRECTION ( 'NONE',  ( 3.295974604355930324E-14, 1.000000000000000000, 0.000000000000000000 ) ) ;
#8211 = CARTESIAN_POINT ( 'NONE',  ( 22.61475049040999963, 10.14616672796000074, -1.561894924173000243 ) ) ;
#8212 = EDGE_CURVE ( 'NONE', #21190, #13265, #8522, .T. ) ;
#8213 = CARTESIAN_POINT ( 'NONE',  ( 14.74679166666666674, -9.049713451602187320, -1.184477773038146831 ) ) ;
#8214 = ORIENTED_EDGE ( 'NONE', *, *, #6136, .T. ) ;
#8215 = CARTESIAN_POINT ( 'NONE',  ( -1.989999999999999991, 9.799994897958001161, -7.500000000000000000 ) ) ;
#8216 = CARTESIAN_POINT ( 'NONE',  ( -2.096579189799000265, 28.03956776952000141, 1.652809762273000027 ) ) ;
#8217 = VECTOR ( 'NONE', #1854, 1000.000000000000000 ) ;
#8218 = CARTESIAN_POINT ( 'NONE',  ( -4.509512206469002749, 12.45276351814001536, 1.421174038937999873 ) ) ;
#8219 = CARTESIAN_POINT ( 'NONE',  ( 2.085423526801265748, 28.97009402253615917, 0.5636491508442302845 ) ) ;
#8220 = CARTESIAN_POINT ( 'NONE',  ( 0.04809324771324000047, 27.21687716035999927, 2.449054215377000077 ) ) ;
#8221 = CARTESIAN_POINT ( 'NONE',  ( 10.35615758860000035, -7.000000000000000000, 0.000000000000000000 ) ) ;
#8222 = ORIENTED_EDGE ( 'NONE', *, *, #2389, .T. ) ;
#8223 = CARTESIAN_POINT ( 'NONE',  ( -24.43506354683020731, 1.794296882888009259, -12.50003182001805868 ) ) ;
#8224 = CARTESIAN_POINT ( 'NONE',  ( 0.5551539414043799026, 26.26248452079970619, 2.089084675604010233 ) ) ;
#8225 = DIRECTION ( 'NONE',  ( 0.000000000000000000, 1.000000000000000000, 0.000000000000000000 ) ) ;
#8226 = CARTESIAN_POINT ( 'NONE',  ( 0.7252905466825813052, 6.815733255002632163, 1.595975169937962956 ) ) ;
#8227 = DIRECTION ( 'NONE',  ( 0.000000000000000000, 0.000000000000000000, 1.000000000000000000 ) ) ;
#8228 = EDGE_CURVE ( 'NONE', #11130, #13776, #15761, .T. ) ;
#8229 = ADVANCED_FACE ( 'NONE', ( #19539 ), #19274, .F. ) ;
#8230 = CARTESIAN_POINT ( 'NONE',  ( -17.70843032205999990, -8.525337246235000777, 7.569901604118999927 ) ) ;
#8231 = CIRCLE ( 'NONE', #109, 2.099999992707999308 ) ;
#8232 = CARTESIAN_POINT ( 'NONE',  ( 17.97356375731000000, 4.354347264933000616, 8.156255255558999551 ) ) ;
#8233 = CARTESIAN_POINT ( 'NONE',  ( 2.434931691670791931, 27.56666666666666643, 0.6543697108981911814 ) ) ;
#8234 = EDGE_LOOP ( 'NONE', ( #14468, #8922, #19583, #10135 ) ) ;
#8235 = CARTESIAN_POINT ( 'NONE',  ( 18.97016382330117068, -5.824115247012692897, 8.721741054822143013 ) ) ;
#8236 = DIRECTION ( 'NONE',  ( -1.000000000000000000, 0.000000000000000000, 0.000000000000000000 ) ) ;
#8237 = CARTESIAN_POINT ( 'NONE',  ( -15.35178743917333577, 5.570923026602933703, 7.249260680724361805 ) ) ;
#8238 = CARTESIAN_POINT ( 'NONE',  ( 2.459493327843513821, 13.98625086743180823, -5.610299872167907154 ) ) ;
#8239 = ORIENTED_EDGE ( 'NONE', *, *, #22821, .F. ) ;
#8240 = CARTESIAN_POINT ( 'NONE',  ( 4.660957651440996052, 13.44002737945000625, -5.344716610742998419 ) ) ;
#8241 = ADVANCED_FACE ( 'NONE', ( #14669 ), #18495, .T. ) ;
#8242 = CARTESIAN_POINT ( 'NONE',  ( 11.18574820342087506, 1.750427062276028067, 12.50001947252512657 ) ) ;
#8243 = ADVANCED_FACE ( 'NONE', ( #5354 ), #14619, .T. ) ;
#8244 = CARTESIAN_POINT ( 'NONE',  ( 16.70595452243934886, 8.597629843446766174, 5.888985926558585327 ) ) ;
#8245 = CARTESIAN_POINT ( 'NONE',  ( -14.25243324638999809, -13.93375672974000068, 0.8660254037843999608 ) ) ;
#8246 = CARTESIAN_POINT ( 'NONE',  ( 0.000000000000000000, 18.00000000000000000, 0.000000000000000000 ) ) ;
#8247 = CARTESIAN_POINT ( 'NONE',  ( 2.500000000000000000, 29.43419673618999965, 0.000000000000000000 ) ) ;
#8248 = VERTEX_POINT ( 'NONE', #23869 ) ;
#8249 = DIRECTION ( 'NONE',  ( 0.000000000000000000, 1.000000000000000000, 0.000000000000000000 ) ) ;
#8250 = CARTESIAN_POINT ( 'NONE',  ( -1.258584843124999963, 24.77728268470999851, 1.988370622766999940 ) ) ;
#8251 = CARTESIAN_POINT ( 'NONE',  ( 1.142577977447108317, 24.50000000000001066, -2.156693640880154472 ) ) ;
#8252 = ORIENTED_EDGE ( 'NONE', *, *, #21817, .T. ) ;
#8253 = PRODUCT_DEFINITION_SHAPE ( 'NONE', 'NONE',  #2198 ) ;
#8254 = FACE_OUTER_BOUND ( 'NONE', #2787, .T. ) ;
#8255 = CARTESIAN_POINT ( 'NONE',  ( 0.6543697108982239330, 28.46753006952333109, 2.434931691670783049 ) ) ;
#8256 = CARTESIAN_POINT ( 'NONE',  ( -3.967402132374007628, 13.32802061695993245, 5.543097348091962751 ) ) ;
#8257 = CARTESIAN_POINT ( 'NONE',  ( 13.56906889882999856, 3.897513013205000210, 9.769895226178999081 ) ) ;
#8258 = FACE_BOUND ( 'NONE', #4632, .T. ) ;
#8259 = CARTESIAN_POINT ( 'NONE',  ( -6.518352534450451152, 15.19362126070188701, 2.752148752140309629 ) ) ;
#8260 = ORIENTED_EDGE ( 'NONE', *, *, #19284, .T. ) ;
#8261 = ORIENTED_EDGE ( 'NONE', *, *, #18126, .T. ) ;
#8262 = CARTESIAN_POINT ( 'NONE',  ( -13.99999999999999822, -1.124839544070808994, -9.501924303252614834 ) ) ;
#8263 = B_SPLINE_CURVE_WITH_KNOTS ( 'NONE', 3,
 ( #10498, #21275, #1284, #4684, #21633, #4923, #15916, #5052, #12308, #8669, #17998, #19454, #2982, #16036, #1403, #22944, #3351, #14812, #23907, #3576, #16283, #3688, #12664, #7084, #14360, #18463, #20403, #21866, #12779, #8917, #1528, #23788, #9142, #7196, #16638, #3809, #9262, #1875, #14586, #47, #7315 ),
 .UNSPECIFIED., .F., .F.,
 ( 4, 2, 2, 2, 2, 1, 1, 1, 2, 2, 2, 2, 1, 2, 2, 2, 1, 2, 2, 2, 2, 2, 4 ),
 ( 0.000000000000000000, 0.1249999999999944489, 0.2499999999999888978, 0.3749999999999833467, 0.4374999999999805156, 0.4687499999999791278, 0.4843749999999784617, 0.4921874999999780731, 0.4960937499999777955, 0.4999999999999775180, 0.6249999999999618083, 0.6874999999999540368, 0.7187499999999502620, 0.7343749999999485967, 0.7499999999999470424, 0.8124999999999422684, 0.8437499999999414912, 0.8593749999999420464, 0.8749999999999427125, 0.9062499999999577005, 0.9218749999999646949, 0.9374999999999718003, 1.000000000000000000 ),
 .UNSPECIFIED. ) ;
#8264 = DIRECTION ( 'NONE',  ( -1.000000000000000000, 0.000000000000000000, 0.000000000000000000 ) ) ;
#8265 = CARTESIAN_POINT ( 'NONE',  ( 3.099999776787000005, 16.99999977679100027, 5.570936506502000395E-07 ) ) ;
#8266 = ORIENTED_EDGE ( 'NONE', *, *, #13024, .T. ) ;
#8267 = CARTESIAN_POINT ( 'NONE',  ( -22.51591334142999656, -4.717617794095999351, 8.470232659896000271 ) ) ;
#8268 = CARTESIAN_POINT ( 'NONE',  ( 1.717851791802367689, 12.95712093925186181, -1.058657081467656802 ) ) ;
#8269 = CARTESIAN_POINT ( 'NONE',  ( 6.225893253368866453, 13.76032292270264357, 1.310517586579727389 ) ) ;
#8270 = CARTESIAN_POINT ( 'NONE',  ( 15.10228429232423686, 8.300904500292098476, 6.166654416055827426 ) ) ;
#8271 = CARTESIAN_POINT ( 'NONE',  ( -16.35741097668999799, -1.834076948381999861, 10.90256368047000102 ) ) ;
#8272 = CARTESIAN_POINT ( 'NONE',  ( 1.346439123301719665, 24.53198827073828170, 3.841100253455552060 ) ) ;
#8273 = CARTESIAN_POINT ( 'NONE',  ( -20.58725639707271071, 7.574229625886635731, -7.286258484127539070 ) ) ;
#8274 = CONICAL_SURFACE ( 'NONE', #11741, 9.152445778720998959, 0.02565634000431304615 ) ;
#8275 = CARTESIAN_POINT ( 'NONE',  ( 0.000000000000000000, 24.49999999999999645, 0.000000000000000000 ) ) ;
#8276 = CONICAL_SURFACE ( 'NONE', #15597, 4.309401076758999416, 1.119376321708719590 ) ;
#8277 = CARTESIAN_POINT ( 'NONE',  ( -0.7226321071931195439, 29.56039541046514074, 2.038962400747685866 ) ) ;
#8278 = VERTEX_POINT ( 'NONE', #12399 ) ;
#8279 = CARTESIAN_POINT ( 'NONE',  ( 1.160309977445999952, 24.68774815733999972, 2.042291732285999917 ) ) ;
#8280 = CARTESIAN_POINT ( 'NONE',  ( -17.15435783830565342, 1.323833875474687449, -10.33990276428391120 ) ) ;
#8281 = EDGE_LOOP ( 'NONE', ( #21782, #16114, #12047 ) ) ;
#8282 = CARTESIAN_POINT ( 'NONE',  ( 5.985422941791000540, 14.10050748988999558, -1.093390217131999353 ) ) ;
#8283 = CARTESIAN_POINT ( 'NONE',  ( 1.672509921849822945, 28.00639765414753413, 3.652834497693414839 ) ) ;
#8284 = CARTESIAN_POINT ( 'NONE',  ( 4.000000000000000000, 28.00000000000000000, 2.309401076759000304 ) ) ;
#8285 = AXIS2_PLACEMENT_3D ( 'NONE', #10194, #23132, #11890 ) ;
#8286 = CARTESIAN_POINT ( 'NONE',  ( 11.63812642131000175, -9.225545160481999574, -2.612645831888999570 ) ) ;
#8287 = ORIENTED_EDGE ( 'NONE', *, *, #16205, .T. ) ;
#8288 = CARTESIAN_POINT ( 'NONE',  ( -11.53829899291999794, 13.73725242156000093, 4.695599082074999764 ) ) ;
#8289 = DIRECTION ( 'NONE',  ( 0.000000000000000000, 0.000000000000000000, -1.000000000000000000 ) ) ;
#8290 = DIRECTION ( 'NONE',  ( 0.000000000000000000, 1.000000000000000000, 0.000000000000000000 ) ) ;
#8291 = ORIENTED_EDGE ( 'NONE', *, *, #18417, .T. ) ;
#8292 = DIRECTION ( 'NONE',  ( 0.000000000000000000, 1.000000000000000000, 0.000000000000000000 ) ) ;
#8293 = CARTESIAN_POINT ( 'NONE',  ( 11.97297107869419897, 8.401874682668008631, 10.44762502811753180 ) ) ;
#8294 = CIRCLE ( 'NONE', #21456, 10.59999999999999964 ) ;
#8295 = FACE_OUTER_BOUND ( 'NONE', #23383, .T. ) ;
#8296 = CARTESIAN_POINT ( 'NONE',  ( 4.000000000000000888, 26.50000000000000711, 0.1857058784358716907 ) ) ;
#8297 = CARTESIAN_POINT ( 'NONE',  ( 18.32220535724285426, 7.467675211945433489, -7.265422928116811896 ) ) ;
#8298 = CARTESIAN_POINT ( 'NONE',  ( 12.00000000000000178, -4.492900714930693873, -8.522325693148694370 ) ) ;
#8299 = CARTESIAN_POINT ( 'NONE',  ( -14.48875658296588753, -11.47331197282441195, 5.127631166282722752 ) ) ;
#8300 = CARTESIAN_POINT ( 'NONE',  ( 23.72187345334999975, 10.71010072308000005, -3.583216764283999822 ) ) ;
#8301 = CARTESIAN_POINT ( 'NONE',  ( -0.8020744510286262896, 26.50000000000000355, 2.262007200476410684 ) ) ;
#8302 = CARTESIAN_POINT ( 'NONE',  ( -4.238876225541293508, 13.65117341093445447, -4.928522908460266194 ) ) ;
#8303 = CARTESIAN_POINT ( 'NONE',  ( 0.000000000000000000, 24.65000000000000213, 0.000000000000000000 ) ) ;
#8304 = CARTESIAN_POINT ( 'NONE',  ( -1.585299566500308455, 30.10873184028566740, -1.466893546891119948 ) ) ;
#8305 = VERTEX_POINT ( 'NONE', #12511 ) ;
#8306 = CARTESIAN_POINT ( 'NONE',  ( 22.35278487464000108, -9.885260220390001962, 3.173618722452000274 ) ) ;
#8307 = CARTESIAN_POINT ( 'NONE',  ( 24.27152284451553044, 5.868235163808240173, 8.859447828480986331 ) ) ;
#8308 = DIRECTION ( 'NONE',  ( 0.000000000000000000, 0.8660254037844288266, 0.5000000000000169864 ) ) ;
#8309 = EDGE_CURVE ( 'NONE', #9702, #1360, #16366, .T. ) ;
#8310 = CARTESIAN_POINT ( 'NONE',  ( -20.26940516530154213, 9.853058826522531177, -3.638643124395733341 ) ) ;
#8311 = CARTESIAN_POINT ( 'NONE',  ( 23.01485185659291233, 35.51856778792605240, 2.673746900119610359 ) ) ;
#8312 = CARTESIAN_POINT ( 'NONE',  ( 4.802957578314003051, 12.39660239800000241, -1.097938175032000307 ) ) ;
#8313 = ORIENTED_EDGE ( 'NONE', *, *, #21412, .F. ) ;
#8314 = CARTESIAN_POINT ( 'NONE',  ( -15.61892936444682434, -10.51941959121331038, -0.4572010232798279783 ) ) ;
#8315 = CARTESIAN_POINT ( 'NONE',  ( 0.000000000000000000, 9.100092063578999912, 0.000000000000000000 ) ) ;
#8316 = CARTESIAN_POINT ( 'NONE',  ( 0.1384749747861074853, 27.42162562388985947, -2.167302550213716206 ) ) ;
#8317 = APPLICATION_PROTOCOL_DEFINITION ( 'draft international standard', 'automotive_design', 1998, #3108 ) ;
#8318 = CARTESIAN_POINT ( 'NONE',  ( -14.44633172592052439, -2.842506014212291987, -12.49999152948489822 ) ) ;
#8319 = ADVANCED_FACE ( 'NONE', ( #5472 ), #21763, .F. ) ;
#8320 = EDGE_LOOP ( 'NONE', ( #5118, #8261, #1999, #16284 ) ) ;
#8321 = CARTESIAN_POINT ( 'NONE',  ( -10.35615758860000035, 0.000000000000000000, 0.000000000000000000 ) ) ;
#8322 = CARTESIAN_POINT ( 'NONE',  ( 12.32268908530999951, 2.255737295330999981, -9.860771559977997924 ) ) ;
#8323 = CARTESIAN_POINT ( 'NONE',  ( -24.16753210339999924, 10.61389120149999954, 1.426895337364999961 ) ) ;
#8324 = CARTESIAN_POINT ( 'NONE',  ( -19.35159018418999821, 4.683906058243999304, -9.258484707686999826 ) ) ;
#8325 = CARTESIAN_POINT ( 'NONE',  ( -6.012804651762005292, 16.12591231748002585, 0.9718674177908998013 ) ) ;
#8326 = CARTESIAN_POINT ( 'NONE',  ( 14.65187451745999958, -8.945410793015000195, 3.774998133422999835 ) ) ;
#8327 = CARTESIAN_POINT ( 'NONE',  ( -1.281400481305768446, 28.72500111167598291, 1.780029602772844166 ) ) ;
#8328 = PLANE ( 'NONE',  #2294 ) ;
#8329 = CARTESIAN_POINT ( 'NONE',  ( 24.38510397947347386, -9.380175294669545139, 8.753059805729597187 ) ) ;
#8330 = ORIENTED_EDGE ( 'NONE', *, *, #333, .T. ) ;
#8331 = CARTESIAN_POINT ( 'NONE',  ( 1.117133862669296374, 13.75138444617590494, 6.024180917838062754 ) ) ;
#8332 = CARTESIAN_POINT ( 'NONE',  ( -0.7249434865795999494, 26.29250240010000184, -2.778011591584000239 ) ) ;
#8333 = AXIS2_PLACEMENT_3D ( 'NONE', #4615, #19260, #8130 ) ;
#8334 = CARTESIAN_POINT ( 'NONE',  ( 0.7982728184027000351, 11.57868860898998697, 4.682032524405000729 ) ) ;
#8335 = DIRECTION ( 'NONE',  ( -1.421085471520000159E-14, 1.000000000000000000, 0.000000000000000000 ) ) ;
#8336 = ADVANCED_FACE ( 'NONE', ( #719 ), #8055, .F. ) ;
#8337 = CARTESIAN_POINT ( 'NONE',  ( -24.58855165213000404, -0.7745665798849999950, -11.14856580036999922 ) ) ;
#8338 = CARTESIAN_POINT ( 'NONE',  ( -6.838539683295000060, 15.31903503039000114, -1.878299264234999821 ) ) ;
#8339 = EDGE_LOOP ( 'NONE', ( #14248, #16203, #23662, #189, #17166, #8065, #10703 ) ) ;
#8340 = DIRECTION ( 'NONE',  ( -1.000000000000000000, 0.000000000000000000, 0.000000000000000000 ) ) ;
#8341 = CARTESIAN_POINT ( 'NONE',  ( 4.749997698793337442, 12.55003977317844566, 0.6286408267609251421 ) ) ;
#8342 = CARTESIAN_POINT ( 'NONE',  ( -3.950437602410003191, 13.96089141542000966, 4.598127338115999940 ) ) ;
#8343 = CARTESIAN_POINT ( 'NONE',  ( 0.2887885109354977331, 6.783830813142102123, 1.726165157609700129 ) ) ;
#8344 = CARTESIAN_POINT ( 'NONE',  ( 2.749999993363999806, 22.20000000663619844, -7.185653629187000299E-09 ) ) ;
#8345 = CIRCLE ( 'NONE', #3709, 7.000000000000000000 ) ;
#8346 = ADVANCED_FACE ( 'NONE', ( #11639 ), #22358, .T. ) ;
#8347 = CARTESIAN_POINT ( 'NONE',  ( 2.500000000000000000, 27.03419673618999752, 0.000000000000000000 ) ) ;
#8348 = CARTESIAN_POINT ( 'NONE',  ( -19.33347310582000134, -11.41588003357999881, 0.8201876405482001475 ) ) ;
#8349 = AXIS2_PLACEMENT_3D ( 'NONE', #5508, #16523, #11439 ) ;
#8350 = CARTESIAN_POINT ( 'NONE',  ( 13.14731375731000007, -9.095564035174998452, -0.6525005121013000009 ) ) ;
#8351 = LINE ( 'NONE', #4602, #16318 ) ;
#8352 = EDGE_LOOP ( 'NONE', ( #14725, #22676, #7404, #18129 ) ) ;
#8353 = CARTESIAN_POINT ( 'NONE',  ( -22.73956496715868880, 8.318781100009532636, 4.101902574965182069 ) ) ;
#8354 = CARTESIAN_POINT ( 'NONE',  ( -1.013429452669000197, 30.50215507907999779, 2.321226178608000179 ) ) ;
#8355 = DIRECTION ( 'NONE',  ( 1.000000000000000000, 0.000000000000000000, 0.000000000000000000 ) ) ;
#8356 = CARTESIAN_POINT ( 'NONE',  ( -2.029239291679416635, 13.89258580265481235, -5.780038728331018838 ) ) ;
#8357 = ORIENTED_EDGE ( 'NONE', *, *, #21465, .T. ) ;
#8358 = EDGE_CURVE ( 'NONE', #20706, #13184, #8127, .T. ) ;
#8359 = DIRECTION ( 'NONE',  ( 0.000000000000000000, 1.000000000000000000, 0.000000000000000000 ) ) ;
#8360 = FACE_OUTER_BOUND ( 'NONE', #23175, .T. ) ;
#8361 = CARTESIAN_POINT ( 'NONE',  ( -4.750000000000000000, 17.00000000000000000, 0.000000000000000000 ) ) ;
#8362 = CARTESIAN_POINT ( 'NONE',  ( -23.96984461759712914, -0.1669632017148305891, 9.795628538752165326 ) ) ;
#8363 = CARTESIAN_POINT ( 'NONE',  ( 14.89393665860769644, 8.649210458500339982, 5.983929458265615509 ) ) ;
#8364 = CARTESIAN_POINT ( 'NONE',  ( -4.316401441148448370, 13.60025622239311183, 4.968485032647479649 ) ) ;
#8365 = LINE ( 'NONE', #6546, #6141 ) ;
#8366 = ADVANCED_FACE ( 'NONE', ( #20956 ), #6656, .F. ) ;
#8367 = CARTESIAN_POINT ( 'NONE',  ( -24.49594166687720076, -10.56920153270462137, 6.693539566615260838 ) ) ;
#8368 = ORIENTED_EDGE ( 'NONE', *, *, #3479, .F. ) ;
#8369 = CARTESIAN_POINT ( 'NONE',  ( -24.50000000000000000, -9.995791495354000133, -2.484784171996999635 ) ) ;
#8370 = ADVANCED_FACE ( 'NONE', ( #15367 ), #1500, .T. ) ;
#8371 = AXIS2_PLACEMENT_3D ( 'NONE', #3263, #18034, #19491 ) ;
#8372 = CARTESIAN_POINT ( 'NONE',  ( 11.32654380053060983, -9.540497826126133063, 8.475313523054548881 ) ) ;
#8373 = B_SPLINE_CURVE_WITH_KNOTS ( 'NONE', 3,
 ( #20398, #16392, #23554, #3571, #23901, #3683, #11073, #14580 ),
 .UNSPECIFIED., .F., .F.,
 ( 4, 2, 2, 4 ),
 ( 0.000000000000000000, 0.2500000000000000555, 0.5000000000000000000, 1.000000000000000000 ),
 .UNSPECIFIED. ) ;
#8374 = VERTEX_POINT ( 'NONE', #11755 ) ;
#8375 = CARTESIAN_POINT ( 'NONE',  ( 2.676712279640000247, 26.03320613874000244, 0.5717015712084999590 ) ) ;
#8376 = CARTESIAN_POINT ( 'NONE',  ( -1.764527535379162293, 23.88508205627838521, 1.302939369652649448 ) ) ;
#8377 = CARTESIAN_POINT ( 'NONE',  ( -0.1474219169056815992, 12.80217572131716786, 6.666258639218459514 ) ) ;
#8378 = DIRECTION ( 'NONE',  ( -1.000000000000000000, 0.000000000000000000, 0.000000000000000000 ) ) ;
#8379 = CARTESIAN_POINT ( 'NONE',  ( -5.514248749579007125, 15.59707654392000009, -2.503767479304998211 ) ) ;
#8380 = CARTESIAN_POINT ( 'NONE',  ( 24.43449445986660606, -2.200516184495610261, -12.50000000000000533 ) ) ;
#8381 = EDGE_CURVE ( 'NONE', #8876, #23352, #4586, .T. ) ;
#8382 = VECTOR ( 'NONE', #2902, 1000.000000000000114 ) ;
#8383 = ORIENTED_EDGE ( 'NONE', *, *, #16502, .T. ) ;
#8384 = ADVANCED_FACE ( 'NONE', ( #962 ), #21072, .F. ) ;
#8385 = DIRECTION ( 'NONE',  ( 0.000000000000000000, -1.000000000000000000, 0.000000000000000000 ) ) ;
#8386 = CARTESIAN_POINT ( 'NONE',  ( 7.500000000000000000, -9.000000000000000000, 0.000000000000000000 ) ) ;
#8387 = LINE ( 'NONE', #1113, #10622 ) ;
#8388 = ORIENTED_EDGE ( 'NONE', *, *, #14178, .F. ) ;
#8389 = CARTESIAN_POINT ( 'NONE',  ( -19.33246705848000246, 1.882390077888999924, 9.955257576596000746 ) ) ;
#8390 = DIRECTION ( 'NONE',  ( 0.000000000000000000, 1.000000000000000000, 0.000000000000000000 ) ) ;
#8391 = VECTOR ( 'NONE', #2077, 1000.000000000000000 ) ;
#8392 = CARTESIAN_POINT ( 'NONE',  ( 0.000000000000000000, 28.30000000000000071, -4.618802153517000519 ) ) ;
#8393 = CARTESIAN_POINT ( 'NONE',  ( 15.18172000152949863, 6.262995747030510429, 8.229460703160327739 ) ) ;
#8394 = CARTESIAN_POINT ( 'NONE',  ( -16.53807429171999743, 4.901486691287000319, 9.915372413262000251 ) ) ;
#8395 = DIRECTION ( 'NONE',  ( 0.000000000000000000, 0.9345904067404111615, 0.3557256971724040429 ) ) ;
#8396 = CARTESIAN_POINT ( 'NONE',  ( -23.09420251723851436, 9.025778557754042808, 2.425918757917022717 ) ) ;
#8397 = CARTESIAN_POINT ( 'NONE',  ( 3.119669807900996794, 11.98921412105999451, -3.586056005240998878 ) ) ;
#8398 = CARTESIAN_POINT ( 'NONE',  ( -23.86804861157608570, -2.127868428593957528, -9.475271987823031594 ) ) ;
#8399 = CARTESIAN_POINT ( 'NONE',  ( -2.058542572094083756, 29.36339098118925151, -0.6772705394161806502 ) ) ;
#8400 = ORIENTED_EDGE ( 'NONE', *, *, #13967, .F. ) ;
#8401 = VECTOR ( 'NONE', #17139, 1000.000000000000000 ) ;
#8402 = CARTESIAN_POINT ( 'NONE',  ( -0.9500571175814802594, 24.08332894998783758, -2.348467497242777480 ) ) ;
#8403 = CARTESIAN_POINT ( 'NONE',  ( -17.09647949060887839, 3.353307371398061676, -9.871714640295524035 ) ) ;
#8404 = CONICAL_SURFACE ( 'NONE', #13016, 4.309401076758999416, 1.119376321708719590 ) ;
#8405 = EDGE_LOOP ( 'NONE', ( #12364, #14935, #8602, #10044 ) ) ;
#8406 = CARTESIAN_POINT ( 'NONE',  ( 2.000000000000000000, 23.50000000000000000, 0.000000000000000000 ) ) ;
#8407 = CARTESIAN_POINT ( 'NONE',  ( 5.267543338792999741, 14.75420436295999593, -3.146379728334001591 ) ) ;
#8408 = CARTESIAN_POINT ( 'NONE',  ( 2.000000000000000000, 28.00000000000000000, 3.464101615137999968 ) ) ;
#8409 = VECTOR ( 'NONE', #9207, 1000.000000000000114 ) ;
#8410 = PLANE ( 'NONE',  #4922 ) ;
#8411 = CARTESIAN_POINT ( 'NONE',  ( 16.02562642131000104, 9.437180554902999674, -2.258696805882000280 ) ) ;
#8412 = VERTEX_POINT ( 'NONE', #4484 ) ;
#8413 = CARTESIAN_POINT ( 'NONE',  ( 2.053005267516999902E-14, 28.63049582772000079, 2.160000000000000142 ) ) ;
#8414 = CARTESIAN_POINT ( 'NONE',  ( 1.536366799937286087, 26.91666666666666785, -1.999167105995451665 ) ) ;
#8415 = CARTESIAN_POINT ( 'NONE',  ( -5.194121241777001075, 0.000000000000000000, 0.000000000000000000 ) ) ;
#8416 = VERTEX_POINT ( 'NONE', #8361 ) ;
#8417 = CARTESIAN_POINT ( 'NONE',  ( -2.239152124149412781, 24.66084788045843723, 0.1975086853543606968 ) ) ;
#8418 = CARTESIAN_POINT ( 'NONE',  ( 11.78924557932676009, 12.98180138941334505, 2.514846131752552338 ) ) ;
#8419 = CARTESIAN_POINT ( 'NONE',  ( 24.50000000000000000, -10.82531754731000007, -6.250000000000000000 ) ) ;
#8420 = CARTESIAN_POINT ( 'NONE',  ( -3.643546194520564274, 26.29977277844447414, 2.515199777306226903 ) ) ;
#8421 = CARTESIAN_POINT ( 'NONE',  ( 16.75103797537850525, 10.37411370639572006, 0.7522199250260709347 ) ) ;
#8422 = TOROIDAL_SURFACE ( 'NONE', #23486, 14.44999999999999929, 3.850000000000000089 ) ;
#8423 = CARTESIAN_POINT ( 'NONE',  ( 0.000000000000000000, 24.29999999999999716, 0.000000000000000000 ) ) ;
#8424 = CARTESIAN_POINT ( 'NONE',  ( -14.32799115970092885, -8.244301755411107990, 10.71998578050885342 ) ) ;
#8425 = CARTESIAN_POINT ( 'NONE',  ( 20.78512204588000145, -5.382056054770000486, 9.836912527567999831 ) ) ;
#8426 = DIRECTION ( 'NONE',  ( 0.000000000000000000, 1.000000000000000000, 0.000000000000000000 ) ) ;
#8427 = CARTESIAN_POINT ( 'NONE',  ( 2.000000000000000000, 26.50000000000000355, 3.464101615137999968 ) ) ;
#8428 = CARTESIAN_POINT ( 'NONE',  ( 0.000000000000000000, 28.15000000000000213, 0.000000000000000000 ) ) ;
#8429 = CARTESIAN_POINT ( 'NONE',  ( -2.134590991208236144, 30.18387669342094526, -0.3366029040113500681 ) ) ;
#8430 = ORIENTED_EDGE ( 'NONE', *, *, #6414, .T. ) ;
#8431 = CARTESIAN_POINT ( 'NONE',  ( -16.78787077250666471, -5.593750281246704148, 7.278551054825675770 ) ) ;
#8432 = CARTESIAN_POINT ( 'NONE',  ( 21.77303207396000317, 7.050465134612999840, 7.599247105520000822 ) ) ;
#8433 = DIRECTION ( 'NONE',  ( 0.000000000000000000, 1.000000000000000000, 0.000000000000000000 ) ) ;
#8434 = DIRECTION ( 'NONE',  ( 0.000000000000000000, 1.000000000000000000, 0.000000000000000000 ) ) ;
#8435 = B_SPLINE_CURVE_WITH_KNOTS ( 'NONE', 3,
 ( #7588, #5544, #1913, #9302, #11479 ),
 .UNSPECIFIED., .F., .F.,
 ( 4, 1, 4 ),
 ( 0.000000000000000000, 0.5000000000000000000, 1.000000000000000000 ),
 .UNSPECIFIED. ) ;
#8436 = CARTESIAN_POINT ( 'NONE',  ( -20.83170904073196894, -7.016165085331945939, -7.830041573524264109 ) ) ;
#8437 = CARTESIAN_POINT ( 'NONE',  ( 5.155714003469999973, 13.97328511022999997, 4.008150528822999270 ) ) ;
#8438 = CONICAL_SURFACE ( 'NONE', #13444, 13.23032192316000000, 1.093540295016705466 ) ;
#8439 = CARTESIAN_POINT ( 'NONE',  ( -4.939773666788001449, 12.51246242453999002, -0.3358430895244999825 ) ) ;
#8440 = ORIENTED_EDGE ( 'NONE', *, *, #3775, .T. ) ;
#8441 = CARTESIAN_POINT ( 'NONE',  ( 11.99999999337999945, -7.499999993379000252, -2.839934906228000043E-09 ) ) ;
#8442 = FACE_OUTER_BOUND ( 'NONE', #6818, .T. ) ;
#8443 = CARTESIAN_POINT ( 'NONE',  ( -2.157336997581982274, 26.80523531380421787, -0.4247655906842845441 ) ) ;
#8444 = CONICAL_SURFACE ( 'NONE', #19672, 4.309401076758999416, 1.119376321708719590 ) ;
#8445 = CARTESIAN_POINT ( 'NONE',  ( -23.75856372112281178, -13.93375672973999890, -3.388131789017201356E-17 ) ) ;
#8446 = EDGE_LOOP ( 'NONE', ( #8400, #23749, #9086, #22443 ) ) ;
#8447 = CARTESIAN_POINT ( 'NONE',  ( -18.90096560015167171, -5.540366411277957148, 7.367715573165199316 ) ) ;
#8448 = CARTESIAN_POINT ( 'NONE',  ( 20.15099999999999980, -9.188396088570998543, 0.000000000000000000 ) ) ;
#8449 = CARTESIAN_POINT ( 'NONE',  ( -19.88368419381999885, 1.085734961250999886, 11.05963058004999944 ) ) ;
#8450 = ADVANCED_FACE ( 'NONE', ( #6541 ), #16552, .F. ) ;
#8451 = CARTESIAN_POINT ( 'NONE',  ( -16.44171487522000064, -2.047536459366999573, 10.63496198587999864 ) ) ;
#8452 = CARTESIAN_POINT ( 'NONE',  ( -6.041457567962996045, 15.84603627990999009, 1.061821870320000860 ) ) ;
#8453 = CARTESIAN_POINT ( 'NONE',  ( 13.97431994526000132, 2.388644028223000149, 9.947419169996001287 ) ) ;
#8454 = CARTESIAN_POINT ( 'NONE',  ( 1.578394010650965962, 28.30098268268568162, -1.492322616203947572 ) ) ;
#8455 = AXIS2_PLACEMENT_3D ( 'NONE', #13477, #20525, #7678 ) ;
#8456 = FACE_BOUND ( 'NONE', #10377, .T. ) ;
#8457 = CARTESIAN_POINT ( 'NONE',  ( 0.000000000000000000, 29.84999999328000087, 0.000000000000000000 ) ) ;
#8458 = ORIENTED_EDGE ( 'NONE', *, *, #4339, .F. ) ;
#8459 = CARTESIAN_POINT ( 'NONE',  ( 2.625751113930058001, 14.02718270572971093, 5.534244616725424670 ) ) ;
#8460 = CARTESIAN_POINT ( 'NONE',  ( -1.184521108792000010, 28.41369850838000133, -1.932944458086000017 ) ) ;
#8461 = CARTESIAN_POINT ( 'NONE',  ( -19.73562077250665325, -1.201235969070628462, -9.177736638924091750 ) ) ;
#8462 = AXIS2_PLACEMENT_3D ( 'NONE', #1900, #5530, #6993 ) ;
#8463 = EDGE_CURVE ( 'NONE', #7660, #165, #2012, .T. ) ;
#8464 = CARTESIAN_POINT ( 'NONE',  ( -19.76356277338999945, -4.576085012665999763, 10.05190155114000028 ) ) ;
#8465 = CIRCLE ( 'NONE', #7179, 1.500000000000001332 ) ;
#8466 = CIRCLE ( 'NONE', #22363, 1.000000000000000000 ) ;
#8467 = ORIENTED_EDGE ( 'NONE', *, *, #19152, .T. ) ;
#8468 = CARTESIAN_POINT ( 'NONE',  ( 15.82470603379664631, 8.841066507505132677, -2.376100949146749297 ) ) ;
#8469 = CARTESIAN_POINT ( 'NONE',  ( 2.221750175568519836, 11.69191821601775771, -4.278409862297499089 ) ) ;
#8470 = CARTESIAN_POINT ( 'NONE',  ( 0.8460338033015004644, 12.74950668468000714, 6.434662982751002680 ) ) ;
#8471 = CARTESIAN_POINT ( 'NONE',  ( 0.5931794701136839931, 30.59672703127345272, -2.199405972370846563 ) ) ;
#8472 = CARTESIAN_POINT ( 'NONE',  ( -14.25851234944000012, 6.966019679972999867, 12.06748306006000071 ) ) ;
#8473 = CARTESIAN_POINT ( 'NONE',  ( -9.785194711695000436, -11.76217707223999831, -10.20000493973999944 ) ) ;
#8474 = LINE ( 'NONE', #21555, #9237 ) ;
#8475 = CARTESIAN_POINT ( 'NONE',  ( 16.24500142131000047, 8.402176888622001627, 4.865949138796000106 ) ) ;
#8476 = CARTESIAN_POINT ( 'NONE',  ( -1.259047450927242462, 27.33333333333333925, 2.184465970885648201 ) ) ;
#8477 = CIRCLE ( 'NONE', #1519, 2.500000000000000000 ) ;
#8478 = ADVANCED_FACE ( 'NONE', ( #3042 ), #22734, .T. ) ;
#8479 = VERTEX_POINT ( 'NONE', #21443 ) ;
#8480 = CARTESIAN_POINT ( 'NONE',  ( -22.79626902222570095, 9.013103079406477036, 2.422627045988097194 ) ) ;
#8481 = CARTESIAN_POINT ( 'NONE',  ( -0.9369953447464000051, 30.39672044851000265, 2.146156417431999586 ) ) ;
#8482 = CARTESIAN_POINT ( 'NONE',  ( 10.35615758860000035, 0.000000000000000000, 0.000000000000000000 ) ) ;
#8483 = CARTESIAN_POINT ( 'NONE',  ( -2.000000000000000000, 24.50000000000000000, 3.464101615137999968 ) ) ;
#8484 = AXIS2_PLACEMENT_3D ( 'NONE', #22634, #6413, #9809 ) ;
#8485 = ORIENTED_EDGE ( 'NONE', *, *, #3025, .F. ) ;
#8486 = DIRECTION ( 'NONE',  ( -1.000000000000000000, 0.000000000000000000, 0.000000000000000000 ) ) ;
#8487 = DIRECTION ( 'NONE',  ( 0.000000000000000000, 1.000000000000000000, 0.000000000000000000 ) ) ;
#8488 = CARTESIAN_POINT ( 'NONE',  ( -1.135623862809999940, 29.11990199424000281, 2.499808603183999889 ) ) ;
#8489 = CARTESIAN_POINT ( 'NONE',  ( -23.68078907432000335, -9.459496811531000304, -9.754788243598999975E-09 ) ) ;
#8490 = CARTESIAN_POINT ( 'NONE',  ( 16.90109490777444279, 3.018130821474940273, 9.980111950484205963 ) ) ;
#8491 = CARTESIAN_POINT ( 'NONE',  ( -2.653270836322015214, 24.53198827073824617, 3.086600612158310941 ) ) ;
#8492 = AXIS2_PLACEMENT_3D ( 'NONE', #17081, #19134, #7764 ) ;
#8493 = CARTESIAN_POINT ( 'NONE',  ( -21.88974577250666798, -8.992656465434315294, -2.416839618442697457 ) ) ;
#8494 = ADVANCED_FACE ( 'NONE', ( #64 ), #8444, .T. ) ;
#8495 = LINE ( 'NONE', #12488, #17777 ) ;
#8496 = ORIENTED_EDGE ( 'NONE', *, *, #1089, .F. ) ;
#8497 = DIRECTION ( 'NONE',  ( -1.000000000000000000, 0.000000000000000000, 0.000000000000000000 ) ) ;
#8498 = CARTESIAN_POINT ( 'NONE',  ( -4.622974180749045203, 12.49837193735187668, -1.256033617784199530 ) ) ;
#8499 = VERTEX_POINT ( 'NONE', #19632 ) ;
#8500 = AXIS2_PLACEMENT_3D ( 'NONE', #20313, #3719, #18965 ) ;
#8501 = CARTESIAN_POINT ( 'NONE',  ( -1.583728643957000193, 25.44007955149000111, -1.992425406035000179 ) ) ;
#8502 = CARTESIAN_POINT ( 'NONE',  ( 5.574705741524002001, 14.65050554898000357, 2.561573290176999862 ) ) ;
#8503 = CARTESIAN_POINT ( 'NONE',  ( -3.420654925002923896, 13.19662773910879139, 5.846983118698949156 ) ) ;
#8504 = AXIS2_PLACEMENT_3D ( 'NONE', #10981, #23695, #9287 ) ;
#8505 = CARTESIAN_POINT ( 'NONE',  ( 24.24531177150999994, 0.000000000000000000, 0.000000000000000000 ) ) ;
#8506 = CARTESIAN_POINT ( 'NONE',  ( -20.99098205976333986, 9.020086631983017966, 2.148244413887738791 ) ) ;
#8507 = CONICAL_SURFACE ( 'NONE', #16610, 4.699999872533999756, 0.7853981633972997312 ) ;
#8508 = ADVANCED_FACE ( 'NONE', ( #21689 ), #9214, .T. ) ;
#8509 = LINE ( 'NONE', #23259, #12873 ) ;
#8510 = ORIENTED_EDGE ( 'NONE', *, *, #4184, .T. ) ;
#8511 = CARTESIAN_POINT ( 'NONE',  ( 0.3272492347489454056, 30.05086340285667745, 2.499999999999998668 ) ) ;
#8512 = DIRECTION ( 'NONE',  ( 0.000000000000000000, 0.8660254037844288266, 0.5000000000000169864 ) ) ;
#8513 = APPLICATION_CONTEXT ( 'automotive_design' ) ;
#8514 = CARTESIAN_POINT ( 'NONE',  ( 0.000000000000000000, 8.900000000000000355, 0.000000000000000000 ) ) ;
#8515 = EDGE_CURVE ( 'NONE', #21280, #15589, #12368, .T. ) ;
#8516 = ORIENTED_EDGE ( 'NONE', *, *, #12622, .F. ) ;
#8517 = CARTESIAN_POINT ( 'NONE',  ( -21.97548978617999893, 8.585592753479998507, -6.430155294164999980 ) ) ;
#8518 = EDGE_CURVE ( 'NONE', #6561, #2989, #22249, .T. ) ;
#8519 = DIRECTION ( 'NONE',  ( 0.000000000000000000, 0.000000000000000000, 1.000000000000000000 ) ) ;
#8520 = CARTESIAN_POINT ( 'NONE',  ( 15.14773914344095296, 7.218886667550619585, 7.399516787738322776 ) ) ;
#8521 = FACE_OUTER_BOUND ( 'NONE', #19628, .T. ) ;
#8522 = LINE ( 'NONE', #6445, #1087 ) ;
#8523 = CARTESIAN_POINT ( 'NONE',  ( -12.00000000000000000, 1.371604415045000054E-14, 0.000000000000000000 ) ) ;
#8524 = CARTESIAN_POINT ( 'NONE',  ( 2.325033434249998976, 11.79288290861998334, -4.153457988357001973 ) ) ;
#8525 = ORIENTED_EDGE ( 'NONE', *, *, #11602, .T. ) ;
#8526 = CARTESIAN_POINT ( 'NONE',  ( -23.99443888926111867, -4.202096428969419151, -8.897806421831953472 ) ) ;
#8527 = CARTESIAN_POINT ( 'NONE',  ( -2.053677740305431598, 29.44401705994312479, 0.6690189489189264371 ) ) ;
#8528 = ADVANCED_FACE ( 'NONE', ( #3165 ), #14296, .T. ) ;
#8529 = ORIENTED_EDGE ( 'NONE', *, *, #10279, .F. ) ;
#8530 = CARTESIAN_POINT ( 'NONE',  ( 2.434931691670788823, 29.23333333333333073, -0.6543697108982009514 ) ) ;
#8531 = CARTESIAN_POINT ( 'NONE',  ( -15.53376410279586928, -5.343199712982666938, -8.901057557536040221 ) ) ;
#8532 = VECTOR ( 'NONE', #14517, 1000.000000000000227 ) ;
#8533 = VERTEX_POINT ( 'NONE', #18606 ) ;
#8534 = CARTESIAN_POINT ( 'NONE',  ( 4.820157802215999432, 14.15666734818999650, -4.018441328438997040 ) ) ;
#8535 = CARTESIAN_POINT ( 'NONE',  ( 12.00000000000000355, -3.820038909443681074, -8.126794263889502545 ) ) ;
#8536 = DIRECTION ( 'NONE',  ( -0.5000000000000169864, 0.8660254037844288266, 0.000000000000000000 ) ) ;
#8537 = CARTESIAN_POINT ( 'NONE',  ( 18.71100174931000026, 5.082731606397000057, 9.520742961040999930 ) ) ;
#8538 = EDGE_LOOP ( 'NONE', ( #13973, #5017, #10352, #7142 ) ) ;
#8539 = FACE_OUTER_BOUND ( 'NONE', #6496, .T. ) ;
#8540 = CARTESIAN_POINT ( 'NONE',  ( -24.50000000000000000, 1.524685264937999788E-14, 0.000000000000000000 ) ) ;
#8541 = DIRECTION ( 'NONE',  ( 0.000000000000000000, 1.000000000000000000, 0.000000000000000000 ) ) ;
#8542 = EDGE_CURVE ( 'NONE', #7505, #6250, #16171, .T. ) ;
#8543 = ORIENTED_EDGE ( 'NONE', *, *, #11697, .F. ) ;
#8544 = EDGE_CURVE ( 'NONE', #9739, #7943, #12244, .T. ) ;
#8545 = CARTESIAN_POINT ( 'NONE',  ( 11.18529249867709474, 9.951874339556875171, 7.762889674103440996 ) ) ;
#8546 = FACE_OUTER_BOUND ( 'NONE', #3019, .T. ) ;
#8547 = DIRECTION ( 'NONE',  ( 1.000000000000000000, 0.000000000000000000, 0.000000000000000000 ) ) ;
#8548 = CARTESIAN_POINT ( 'NONE',  ( 16.95399261017279713, 7.433768333657749139, 7.292702827057317982 ) ) ;
#8549 = CARTESIAN_POINT ( 'NONE',  ( 11.99999999999999645, -5.748969532828861695, -7.831912490070881638 ) ) ;
#8550 = DIRECTION ( 'NONE',  ( 1.000000000000000000, 0.000000000000000000, 0.000000000000000000 ) ) ;
#8551 = CARTESIAN_POINT ( 'NONE',  ( -4.294719301634956743, 13.61382386032614100, -4.956612227401347326 ) ) ;
#8552 = CARTESIAN_POINT ( 'NONE',  ( -0.7783053373570000266, 26.50000000000000000, 6.000000000000000000 ) ) ;
#8553 = CARTESIAN_POINT ( 'NONE',  ( -1.143039311806165026, 30.33272233741166701, 1.832923158551177822 ) ) ;
#8554 = ADVANCED_FACE ( 'NONE', ( #17819 ), #9990, .T. ) ;
#8555 = ORIENTED_EDGE ( 'NONE', *, *, #13218, .F. ) ;
#8556 = CARTESIAN_POINT ( 'NONE',  ( 19.26076993769000367, -0.2568395230875999968, -10.29350776803000045 ) ) ;
#8557 = CARTESIAN_POINT ( 'NONE',  ( 23.84592208957456805, 9.371304666163794650, -4.977627156037889300 ) ) ;
#8558 = DIRECTION ( 'NONE',  ( -1.000000000000000000, 0.000000000000000000, 0.000000000000000000 ) ) ;
#8559 = ORIENTED_EDGE ( 'NONE', *, *, #10443, .T. ) ;
#8560 = CARTESIAN_POINT ( 'NONE',  ( 0.000000000000000000, 29.84999999328000087, -2.249999993279999888 ) ) ;
#8561 = CARTESIAN_POINT ( 'NONE',  ( 0.000000000000000000, 22.00000000000000000, 0.000000000000000000 ) ) ;
#8562 = ORIENTED_EDGE ( 'NONE', *, *, #3479, .T. ) ;
#8563 = CARTESIAN_POINT ( 'NONE',  ( -16.31671029517696780, 7.464073496724219048, 7.241521120158354030 ) ) ;
#8564 = DIRECTION ( 'NONE',  ( 0.000000000000000000, 1.000000000000000000, 0.000000000000000000 ) ) ;
#8565 = ORIENTED_EDGE ( 'NONE', *, *, #8309, .F. ) ;
#8566 = CARTESIAN_POINT ( 'NONE',  ( -1.815862101691702479, 26.75592408899736085, -1.190014743604365322 ) ) ;
#8567 = DIRECTION ( 'NONE',  ( 0.000000000000000000, 0.000000000000000000, 1.000000000000000000 ) ) ;
#8568 = DIRECTION ( 'NONE',  ( 0.000000000000000000, 0.000000000000000000, 1.000000000000000000 ) ) ;
#8569 = VERTEX_POINT ( 'NONE', #4857 ) ;
#8570 = CARTESIAN_POINT ( 'NONE',  ( -15.91276253787999728, 9.079634562165001199, 0.000000000000000000 ) ) ;
#8571 = CARTESIAN_POINT ( 'NONE',  ( 1.699986222664000124, 9.100024384209000061, 1.053575639828000066 ) ) ;
#8572 = CARTESIAN_POINT ( 'NONE',  ( -21.48955104351000145, -6.509886382642999791, 9.059949078605001205 ) ) ;
#8573 = CARTESIAN_POINT ( 'NONE',  ( -13.39475965566999882, 9.583002289957001096, -2.464304261457999967 ) ) ;
#8574 = CARTESIAN_POINT ( 'NONE',  ( 22.45629166666665455, 1.210375094748636471, -9.247554416229247565 ) ) ;
#8575 = CARTESIAN_POINT ( 'NONE',  ( 14.44874951745999958, -4.376472204050999792, 8.660696927216999796 ) ) ;
#8576 = FACE_OUTER_BOUND ( 'NONE', #21775, .T. ) ;
#8577 = CARTESIAN_POINT ( 'NONE',  ( 5.302302355349000074, 1.583778078195999810E-14, 0.000000000000000000 ) ) ;
#8578 = CARTESIAN_POINT ( 'NONE',  ( 15.20029166666666320, 1.186001144903479299, -9.061351155403777113 ) ) ;
#8579 = ORIENTED_EDGE ( 'NONE', *, *, #9772, .T. ) ;
#8580 = CARTESIAN_POINT ( 'NONE',  ( -1.182434930542718865, 26.44682129341586574, -3.936123028068912344 ) ) ;
#8581 = DIRECTION ( 'NONE',  ( 0.000000000000000000, -1.000000000000000000, 0.000000000000000000 ) ) ;
#8582 = CARTESIAN_POINT ( 'NONE',  ( 2.254114612530000006, 25.82163313895000201, 0.5071914623444000458 ) ) ;
#8583 = CARTESIAN_POINT ( 'NONE',  ( -19.28212077250665857, 9.166098935122516167, -1.199712597205310871 ) ) ;
#8584 = CARTESIAN_POINT ( 'NONE',  ( 0.5033195914047999819, 28.84187716036000282, 2.236906829057999868 ) ) ;
#8585 = CARTESIAN_POINT ( 'NONE',  ( -4.290394981784330319, 12.24616331916512024, 2.243719369978889322 ) ) ;
#8586 = ORIENTED_EDGE ( 'NONE', *, *, #1649, .F. ) ;
#8587 = CARTESIAN_POINT ( 'NONE',  ( 15.86249770046331165, 9.078344667370600973, -1.188479485729073692 ) ) ;
#8588 = CARTESIAN_POINT ( 'NONE',  ( -24.50000000000000000, 0.000000000000000000, -12.50000000000000000 ) ) ;
#8589 = FACE_OUTER_BOUND ( 'NONE', #4960, .T. ) ;
#8590 = CARTESIAN_POINT ( 'NONE',  ( 1.570131409422825142, 6.957183850560507921, 0.7744548611195164467 ) ) ;
#8591 = CARTESIAN_POINT ( 'NONE',  ( -14.25243324638999809, 6.216878364870000340, 12.50000000000000000 ) ) ;
#8592 = CARTESIAN_POINT ( 'NONE',  ( -0.3272492347488898945, 24.18333333333333357, 2.500000000000005329 ) ) ;
#8593 = CARTESIAN_POINT ( 'NONE',  ( -6.121054384213369559, 15.98142497799454809, -1.054679361892482570 ) ) ;
#8594 = CARTESIAN_POINT ( 'NONE',  ( 16.90312642131000231, -9.179335210403001710, 3.217155551743000164 ) ) ;
#8595 = CARTESIAN_POINT ( 'NONE',  ( 2.500000000000000000, 27.59999999999999787, 0.000000000000000000 ) ) ;
#8596 = AXIS2_PLACEMENT_3D ( 'NONE', #5870, #3591, #13141 ) ;
#8597 = ORIENTED_EDGE ( 'NONE', *, *, #14380, .T. ) ;
#8598 = LINE ( 'NONE', #4974, #5385 ) ;
#8599 = CARTESIAN_POINT ( 'NONE',  ( -2.554677365147000057, 29.61489390254000043, -0.9449442378532999509 ) ) ;
#8600 = CARTESIAN_POINT ( 'NONE',  ( -15.08724577250666776, -2.371147453209594413, 8.822634382605400560 ) ) ;
#8601 = CARTESIAN_POINT ( 'NONE',  ( 3.839343825864000692, 14.39937964873592513, -4.778446983982809648 ) ) ;
#8602 = ORIENTED_EDGE ( 'NONE', *, *, #16321, .F. ) ;
#8603 = CARTESIAN_POINT ( 'NONE',  ( -0.3380190453170119902, 26.50000000000001421, -2.400617273097169768 ) ) ;
#8604 = CARTESIAN_POINT ( 'NONE',  ( 0.000000000000000000, 19.04999994433000055, 0.000000000000000000 ) ) ;
#8605 = CARTESIAN_POINT ( 'NONE',  ( 6.125000094578820331, 14.37502624149403552, 0.003861642916549869620 ) ) ;
#8606 = CARTESIAN_POINT ( 'NONE',  ( 18.75008227645999881, 0.000000000000000000, 0.000000000000000000 ) ) ;
#8607 = CARTESIAN_POINT ( 'NONE',  ( 15.28421742927796778, -4.014701272140648314, 9.733939712514935394 ) ) ;
#8608 = CARTESIAN_POINT ( 'NONE',  ( -4.039176818549614190, 13.81482912323319390, 4.860923934985756034 ) ) ;
#8609 = CARTESIAN_POINT ( 'NONE',  ( -4.695566743926001152, 12.35651713445999178, 1.468545715520999773 ) ) ;
#8610 = CARTESIAN_POINT ( 'NONE',  ( 61.60588651278290939, 35.51856778792605240, 1.000000000000000000 ) ) ;
#8611 = ORIENTED_EDGE ( 'NONE', *, *, #10769, .F. ) ;
#8612 = FACE_OUTER_BOUND ( 'NONE', #570, .T. ) ;
#8613 = CARTESIAN_POINT ( 'NONE',  ( -0.6303327290807835270, 11.57525023284983234, -4.749574817190888254 ) ) ;
#8614 = EDGE_LOOP ( 'NONE', ( #10136, #18868, #20205, #14687 ) ) ;
#8615 = EDGE_CURVE ( 'NONE', #19206, #11018, #11229, .T. ) ;
#8616 = CARTESIAN_POINT ( 'NONE',  ( 2.488989593372999742, 25.92777150816999665, 0.5316071032648000960 ) ) ;
#8617 = CARTESIAN_POINT ( 'NONE',  ( 5.811180458947997174, 14.57924603701000521, 1.966607779951999202 ) ) ;
#8618 = CARTESIAN_POINT ( 'NONE',  ( -0.4299899780664359628, 12.80997083806871828, 6.651184739924561384 ) ) ;
#8619 = VECTOR ( 'NONE', #3426, 999.9999999999998863 ) ;
#8620 = DIRECTION ( 'NONE',  ( -1.000000000000000000, 0.000000000000000000, 0.000000000000000000 ) ) ;
#8621 = CARTESIAN_POINT ( 'NONE',  ( -5.398695926155999025, 16.20485681822998814, -2.910764035052000320 ) ) ;
#8622 = ORIENTED_EDGE ( 'NONE', *, *, #12608, .T. ) ;
#8623 = CARTESIAN_POINT ( 'NONE',  ( 22.35132670216743023, 35.07441746931982607, -6.000000000000005329 ) ) ;
#8624 = CARTESIAN_POINT ( 'NONE',  ( -1.970034741582993298, 26.25401323305582935, 0.8711804643216717325 ) ) ;
#8625 = CYLINDRICAL_SURFACE ( 'NONE', #1683, 7.500000000000000000 ) ;
#8626 = ORIENTED_EDGE ( 'NONE', *, *, #12517, .T. ) ;
#8627 = EDGE_CURVE ( 'NONE', #12256, #4069, #283, .T. ) ;
#8628 = CARTESIAN_POINT ( 'NONE',  ( -21.46138957935999869, 4.494222062375999194, 9.724264673970999695 ) ) ;
#8629 = CARTESIAN_POINT ( 'NONE',  ( -4.750000000000000000, 17.00000000000000000, 0.000000000000000000 ) ) ;
#8630 = CARTESIAN_POINT ( 'NONE',  ( 15.14749159410988888, 7.225522084805205303, 7.393037676230730604 ) ) ;
#8631 = DIRECTION ( 'NONE',  ( -1.000000000000000000, 0.000000000000000000, 0.000000000000000000 ) ) ;
#8632 = CARTESIAN_POINT ( 'NONE',  ( 0.1261743698658000234, 30.29791251314999911, 2.164316091856000046 ) ) ;
#8633 = CARTESIAN_POINT ( 'NONE',  ( -12.24999999459000044, 1.554281285377000029E-14, 1.045589212608000028E-14 ) ) ;
#8634 = CARTESIAN_POINT ( 'NONE',  ( 4.705295477336001397, 12.52895486067000164, -0.5082585761650004752 ) ) ;
#8635 = ORIENTED_EDGE ( 'NONE', *, *, #381, .T. ) ;
#8636 = VECTOR ( 'NONE', #12138, 1000.000000000000227 ) ;
#8637 = CARTESIAN_POINT ( 'NONE',  ( -16.89590893017999562, 5.628454363070000355, -9.888856528401998247 ) ) ;
#8638 = CARTESIAN_POINT ( 'NONE',  ( -0.09735432568101735906, 29.20954443492663444, -2.161772490294577853 ) ) ;
#8639 = VERTEX_POINT ( 'NONE', #6108 ) ;
#8640 = DIRECTION ( 'NONE',  ( -0.000000000000000000, 1.000000000000000000, 0.000000000000000000 ) ) ;
#8641 = CARTESIAN_POINT ( 'NONE',  ( -14.92604145197964804, 10.36539917058194327, -0.05665573055404094643 ) ) ;
#8642 = ORIENTED_EDGE ( 'NONE', *, *, #20575, .T. ) ;
#8643 = EDGE_CURVE ( 'NONE', #4710, #9272, #19665, .T. ) ;
#8644 = CARTESIAN_POINT ( 'NONE',  ( 0.5756525555721964116, 30.79585480968119171, -2.147306472175536385 ) ) ;
#8645 = CARTESIAN_POINT ( 'NONE',  ( 12.00000000000000178, 3.029763647141548777, -8.454266960972679712 ) ) ;
#8646 = CARTESIAN_POINT ( 'NONE',  ( 13.79085740026999929, -10.35098683540000053, -3.711371709585999934 ) ) ;
#8647 = CARTESIAN_POINT ( 'NONE',  ( 0.1453149127350999992, 27.37756359724000177, -2.464088664829000130 ) ) ;
#8648 = CARTESIAN_POINT ( 'NONE',  ( 16.71018908530999880, 2.886377165994000293, 9.815223273854998709 ) ) ;
#8649 = EDGE_LOOP ( 'NONE', ( #18958, #18609, #7777, #19839 ) ) ;
#8650 = CARTESIAN_POINT ( 'NONE',  ( -10.72371899292000030, -11.98290193648999846, -8.195774483354998807 ) ) ;
#8651 = CARTESIAN_POINT ( 'NONE',  ( 13.49999999999999645, 9.153938654719679491, -2.308705407138142540 ) ) ;
#8652 = DIRECTION ( 'NONE',  ( 0.000000000000000000, 0.000000000000000000, -1.000000000000000000 ) ) ;
#8653 = ORIENTED_EDGE ( 'NONE', *, *, #4552, .T. ) ;
#8654 = EDGE_CURVE ( 'NONE', #18916, #5087, #14461, .T. ) ;
#8655 = CARTESIAN_POINT ( 'NONE',  ( 12.06371966925979144, 13.38412994816690293, 1.818205397975688697 ) ) ;
#8656 = CARTESIAN_POINT ( 'NONE',  ( 22.14693913686161864, 8.854242334004002402, 6.059094452743556403 ) ) ;
#8657 = CARTESIAN_POINT ( 'NONE',  ( -14.00000000000000178, 7.941986550240724085, 4.595816627501706719 ) ) ;
#8658 = CARTESIAN_POINT ( 'NONE',  ( 17.21630533617675596, -1.189482518535111666, 10.35523827938461494 ) ) ;
#8659 = BREP_WITH_VOIDS ( 'NONE', #10812, ( #16553, #414, #21897, #7527, #855 ) );
#8660 = FACE_OUTER_BOUND ( 'NONE', #13852, .T. ) ;
#8661 = CARTESIAN_POINT ( 'NONE',  ( -4.750000000000000000, 16.89999999999999858, 0.000000000000000000 ) ) ;
#8662 = CARTESIAN_POINT ( 'NONE',  ( 0.3564538054804341494, 26.29977277844468020, 4.413003452969197049 ) ) ;
#8663 = CARTESIAN_POINT ( 'NONE',  ( -9.042815982636001948, 21.50000000000000000, 1.000000000000000000 ) ) ;
#8664 = CARTESIAN_POINT ( 'NONE',  ( -1.587703551898336896, 30.10893883470173904, -1.464285708681415388 ) ) ;
#8665 = ORIENTED_EDGE ( 'NONE', *, *, #7018, .T. ) ;
#8666 = CARTESIAN_POINT ( 'NONE',  ( 0.9782764959233999358, 25.15935197643999999, -2.120942277036999890 ) ) ;
#8667 = CARTESIAN_POINT ( 'NONE',  ( 11.48478210364012675, 9.189386602319286723, -9.083340531634625847 ) ) ;
#8668 = CARTESIAN_POINT ( 'NONE',  ( -4.544340308300998998, 13.49051417780999884, -5.132142894851999593 ) ) ;
#8669 = CARTESIAN_POINT ( 'NONE',  ( -1.310299540072302538, 23.61517381211949029, -1.660816364045096583 ) ) ;
#8670 = CONICAL_SURFACE ( 'NONE', #921, 4.309401076758999416, 1.119376321708719590 ) ;
#8671 = VERTEX_POINT ( 'NONE', #6604 ) ;
#8672 = EDGE_CURVE ( 'NONE', #11805, #3010, #21970, .T. ) ;
#8673 = CARTESIAN_POINT ( 'NONE',  ( 0.000000000000000000, 16.95000012746599793, -4.699999872533999756 ) ) ;
#8674 = LINE ( 'NONE', #10374, #723 ) ;
#8675 = ADVANCED_FACE ( 'NONE', ( #11943 ), #19327, .T. ) ;
#8676 = DIRECTION ( 'NONE',  ( -1.000000000000000000, 0.000000000000000000, 0.000000000000000000 ) ) ;
#8677 = ORIENTED_EDGE ( 'NONE', *, *, #13069, .T. ) ;
#8678 = CARTESIAN_POINT ( 'NONE',  ( -14.61412482419791559, 9.602449638622033490, 3.892213435086770090 ) ) ;
#8679 = DIRECTION ( 'NONE',  ( 1.000000000000000000, 0.000000000000000000, 0.000000000000000000 ) ) ;
#8680 = VECTOR ( 'NONE', #14194, 1000.000000000000000 ) ;
#8681 = ORIENTED_EDGE ( 'NONE', *, *, #9828, .T. ) ;
#8682 = CARTESIAN_POINT ( 'NONE',  ( 0.9584783449968901081, 26.28746745333229029, 1.979923197800155688 ) ) ;
#8683 = CARTESIAN_POINT ( 'NONE',  ( -14.29262089130156532, -5.684429818840943227, -12.49999999999983658 ) ) ;
#8684 = ORIENTED_EDGE ( 'NONE', *, *, #5853, .F. ) ;
#8685 = EDGE_CURVE ( 'NONE', #8374, #14961, #2618, .T. ) ;
#8686 = LINE ( 'NONE', #19830, #4417 ) ;
#8687 = EDGE_CURVE ( 'NONE', #20918, #20749, #5046, .T. ) ;
#8688 = CARTESIAN_POINT ( 'NONE',  ( -4.096752709992895980, 15.04509484834502686, -4.553272908285909359 ) ) ;
#8689 = B_SPLINE_CURVE_WITH_KNOTS ( 'NONE', 3,
 ( #3705, #533, #7568, #15187, #14947, #7815, #295, #15071, #9285, #22465 ),
 .UNSPECIFIED., .F., .F.,
 ( 4, 1, 1, 2, 2, 4 ),
 ( 0.000000000000000000, 0.2499999999999987788, 0.3749999999999986122, 0.4374999999999987232, 0.4999999999999988898, 1.000000000000000000 ),
 .UNSPECIFIED. ) ;
#8690 = CARTESIAN_POINT ( 'NONE',  ( -21.27697177397000061, -7.986013600915999433, -7.017649059653999544 ) ) ;
#8691 = CARTESIAN_POINT ( 'NONE',  ( -14.00415069958000025, -7.656692200680000226, -7.563137310936999036 ) ) ;
#8692 = DIRECTION ( 'NONE',  ( 0.000000000000000000, -1.000000000000000000, 0.000000000000000000 ) ) ;
#8693 = CARTESIAN_POINT ( 'NONE',  ( 17.90187451746000136, 1.346331495725999972, 9.706975217397999955 ) ) ;
#8694 = CARTESIAN_POINT ( 'NONE',  ( -2.173007427726788343, 27.00242624193079521, -0.03385292825698651975 ) ) ;
#8695 = CARTESIAN_POINT ( 'NONE',  ( 19.69917122382999608, 1.762314512050999982, 8.897469563075999233 ) ) ;
#8696 = DIRECTION ( 'NONE',  ( 0.000000000000000000, 0.000000000000000000, -1.000000000000000000 ) ) ;
#8697 = ORIENTED_EDGE ( 'NONE', *, *, #13248, .T. ) ;
#8698 = CARTESIAN_POINT ( 'NONE',  ( 23.15628936713000030, 9.265517736846000219, 0.000000000000000000 ) ) ;
#8699 = CARTESIAN_POINT ( 'NONE',  ( 0.9482458177890140671, 13.73472448189398953, 6.052214904559278352 ) ) ;
#8700 = CARTESIAN_POINT ( 'NONE',  ( 2.231710853292999897, 28.12119850838000090, 0.3985328791175999918 ) ) ;
#8701 = LINE ( 'NONE', #23463, #18891 ) ;
#8702 = CARTESIAN_POINT ( 'NONE',  ( 24.50000000000000000, 10.82531754731000007, 6.250000000000000000 ) ) ;
#8703 = CARTESIAN_POINT ( 'NONE',  ( -23.58604437744000037, -2.881458659258000043, 10.76926380789999982 ) ) ;
#8704 = AXIS2_PLACEMENT_3D ( 'NONE', #6229, #21009, #4421 ) ;
#8705 = CARTESIAN_POINT ( 'NONE',  ( -2.059536573449531005, 11.66298588225668809, 4.356317206734537706 ) ) ;
#8706 = EDGE_LOOP ( 'NONE', ( #488, #8042, #8510, #6533 ) ) ;
#8707 = DIRECTION ( 'NONE',  ( 1.000000000000000000, 0.000000000000000000, 0.000000000000000000 ) ) ;
#8708 = CARTESIAN_POINT ( 'NONE',  ( -24.46742986863962699, -1.281690452085482379, -12.50000620969121279 ) ) ;
#8709 = CARTESIAN_POINT ( 'NONE',  ( 24.50000000000000000, 8.054858440593999802, 5.882793087032000656 ) ) ;
#8710 = PRESENTATION_LAYER_ASSIGNMENT (  '', '', ( #19537 ) ) ;
#8711 = CARTESIAN_POINT ( 'NONE',  ( 0.000000000000000000, 22.00000000000000000, 0.000000000000000000 ) ) ;
#8712 = ORIENTED_EDGE ( 'NONE', *, *, #3218, .T. ) ;
#8713 = CARTESIAN_POINT ( 'NONE',  ( 13.50000000000000000, -10.65000000000000036, 0.000000000000000000 ) ) ;
#8714 = B_SPLINE_CURVE_WITH_KNOTS ( 'NONE', 3,
 ( #19669, #3319, #16259, #23159, #6578 ),
 .UNSPECIFIED., .F., .F.,
 ( 4, 1, 4 ),
 ( 0.000000000000000000, 0.5000000000000000000, 1.000000000000000000 ),
 .UNSPECIFIED. ) ;
#8715 = CARTESIAN_POINT ( 'NONE',  ( -6.102284808054873722, 16.03473069748903512, -1.037594296848572739 ) ) ;
#8716 = CARTESIAN_POINT ( 'NONE',  ( 13.94156392131000111, 3.761510884484999817, -8.885545664707001023 ) ) ;
#8717 = CARTESIAN_POINT ( 'NONE',  ( 18.52329378839496243, 10.39589489547862478, -0.7791414424835660935 ) ) ;
#8718 = EDGE_LOOP ( 'NONE', ( #1232, #1871, #16398 ) ) ;
#8719 = CARTESIAN_POINT ( 'NONE',  ( 23.41677564524290744, 37.01856778792605240, -6.000000000000000000 ) ) ;
#8720 = CARTESIAN_POINT ( 'NONE',  ( 2.395043234180000091, 29.11238094911999852, 0.8239347788672000128 ) ) ;
#8721 = DIRECTION ( 'NONE',  ( -0.8206518066482797469, 0.5714285714285857187, 0.000000000000000000 ) ) ;
#8722 = CARTESIAN_POINT ( 'NONE',  ( 2.893463358023975029, 14.09696930895991152, -5.402380196813071578 ) ) ;
#8723 = VECTOR ( 'NONE', #3163, 1000.000000000000000 ) ;
#8724 = B_SPLINE_CURVE_WITH_KNOTS ( 'NONE', 3,
 ( #5124, #14326, #13829, #12028, #12270, #2941 ),
 .UNSPECIFIED., .F., .F.,
 ( 4, 1, 1, 4 ),
 ( 0.000000000000000000, 0.3333333333333000081, 0.6666666666667000474, 1.000000000000000000 ),
 .UNSPECIFIED. ) ;
#8725 = ORIENTED_EDGE ( 'NONE', *, *, #11360, .T. ) ;
#8726 = CARTESIAN_POINT ( 'NONE',  ( -0.8905775397556899842, 26.49999999999999289, -2.306335956037367296 ) ) ;
#8727 = LINE ( 'NONE', #10299, #16609 ) ;
#8728 = PRODUCT_DEFINITION ( 'UNKNOWN', '', #19075, #12589 ) ;
#8729 = CARTESIAN_POINT ( 'NONE',  ( 6.124999911758999716, 14.37502625872000195, -0.0001546258496581000123 ) ) ;
#8730 = DIRECTION ( 'NONE',  ( 1.000000000000000000, 0.000000000000000000, 0.000000000000000000 ) ) ;
#8731 = CARTESIAN_POINT ( 'NONE',  ( 15.73025259575829971, -9.722748992816393709, -3.694321794359110012 ) ) ;
#8732 = DIRECTION ( 'NONE',  ( 1.877655941804990996E-08, -0.9999999999999978906, -6.187284376306977451E-08 ) ) ;
#8733 = CARTESIAN_POINT ( 'NONE',  ( 4.820392118736996245, 12.46745978434002033, 1.125972652643999261 ) ) ;
#8734 = CARTESIAN_POINT ( 'NONE',  ( 19.60387270046332731, 8.935620381716546490, 2.401250916706160421 ) ) ;
#8735 = ORIENTED_EDGE ( 'NONE', *, *, #20605, .T. ) ;
#8736 = CARTESIAN_POINT ( 'NONE',  ( -0.003072356603141344206, 30.56339746047213524, 2.483727271772852241 ) ) ;
#8737 = CARTESIAN_POINT ( 'NONE',  ( 23.99062354302999722, -6.216878364870000340, 12.50000000000000000 ) ) ;
#8738 = VERTEX_POINT ( 'NONE', #19812 ) ;
#8739 = CARTESIAN_POINT ( 'NONE',  ( -0.8094216628179000672, 24.22177887107999794, 2.614725727772000408 ) ) ;
#8740 = CARTESIAN_POINT ( 'NONE',  ( 6.082313823887004922, 14.07671881673999970, 0.1102200398116000984 ) ) ;
#8741 = CARTESIAN_POINT ( 'NONE',  ( 11.32654380052724719, -2.569587902914658439, -12.49997024370457588 ) ) ;
#8742 = CIRCLE ( 'NONE', #7949, 4.724999999999999645 ) ;
#8743 = CYLINDRICAL_SURFACE ( 'NONE', #17672, 2.673746900119611247 ) ;
#8744 = CARTESIAN_POINT ( 'NONE',  ( 13.50000000000000178, -1.374339424080784022, 10.20482255197515364 ) ) ;
#8745 = ORIENTED_EDGE ( 'NONE', *, *, #19470, .T. ) ;
#8746 = CARTESIAN_POINT ( 'NONE',  ( -13.99999999999999822, -9.447486684801326362, -3.667138305862581493 ) ) ;
#8747 = FACE_OUTER_BOUND ( 'NONE', #16728, .T. ) ;
#8748 = CARTESIAN_POINT ( 'NONE',  ( -14.25243324638999809, 7.716878364870000340, 11.63397459621999985 ) ) ;
#8749 = ORIENTED_EDGE ( 'NONE', *, *, #16073, .F. ) ;
#8750 = CARTESIAN_POINT ( 'NONE',  ( -21.04613441456000089, -1.628084360272999964, 10.04728532985999934 ) ) ;
#8751 = FACE_BOUND ( 'NONE', #15977, .T. ) ;
#8752 = CARTESIAN_POINT ( 'NONE',  ( 14.89861762386097865, 10.30903294988296004, -0.6934164183026474415 ) ) ;
#8753 = DIRECTION ( 'NONE',  ( 0.000000000000000000, 1.000000000000000000, 0.000000000000000000 ) ) ;
#8754 = EDGE_CURVE ( 'NONE', #15925, #16101, #23772, .T. ) ;
#8755 = SHAPE_REPRESENTATION ( 'Flat Lever Handle', ( #4390 ), #11350 ) ;
#8756 = CARTESIAN_POINT ( 'NONE',  ( -1.812968411601999952, 29.36439700036000033, 1.188835414341000041 ) ) ;
#8757 = DIRECTION ( 'NONE',  ( 0.000000000000000000, 0.000000000000000000, -1.000000000000000000 ) ) ;
#8758 = CARTESIAN_POINT ( 'NONE',  ( -4.297157081715999638, 12.44679617431000551, -2.013149773607997517 ) ) ;
#8759 = ORIENTED_EDGE ( 'NONE', *, *, #13773, .T. ) ;
#8760 = CIRCLE ( 'NONE', #6812, 1.999999999999998668 ) ;
#8761 = CARTESIAN_POINT ( 'NONE',  ( -21.43034587121331569, 8.981271358963487828, -2.413519275972843214 ) ) ;
#8762 = B_SPLINE_CURVE_WITH_KNOTS ( 'NONE', 3,
 ( #4683, #19817, #17634, #2861, #14237, #21750, #12186, #3231 ),
 .UNSPECIFIED., .F., .F.,
 ( 4, 2, 2, 4 ),
 ( 0.000000000000000000, 0.2500000000000002220, 0.5000000000000004441, 1.000000000000000000 ),
 .UNSPECIFIED. ) ;
#8763 = EDGE_LOOP ( 'NONE', ( #23503, #17891, #15346, #11302 ) ) ;
#8764 = CARTESIAN_POINT ( 'NONE',  ( 2.500000000000000000, 29.19999999999999929, 0.000000000000000000 ) ) ;
#8765 = CARTESIAN_POINT ( 'NONE',  ( 0.000000000000000000, 20.10000000000000142, -4.750000000000305533 ) ) ;
#8766 = ORIENTED_EDGE ( 'NONE', *, *, #6801, .T. ) ;
#8767 = CYLINDRICAL_SURFACE ( 'NONE', #20366, 2.500000000000000000 ) ;
#8768 = CARTESIAN_POINT ( 'NONE',  ( 17.39220833333331839, 9.117600057111475920, -1.193618004230062368 ) ) ;
#8769 = EDGE_CURVE ( 'NONE', #14273, #23649, #8373, .T. ) ;
#8770 = CARTESIAN_POINT ( 'NONE',  ( 12.00000000000000355, -6.096004188759242659, -6.621033406203861382 ) ) ;
#8771 = CARTESIAN_POINT ( 'NONE',  ( 18.12167894855999961, 10.39079625826000175, -3.946037309523999781 ) ) ;
#8772 = CARTESIAN_POINT ( 'NONE',  ( -1.675531247043999805, 26.89006359724000106, 1.812579491195999815 ) ) ;
#8773 = ORIENTED_EDGE ( 'NONE', *, *, #7395, .T. ) ;
#8774 = CIRCLE ( 'NONE', #22663, 13.77250448649000525 ) ;
#8775 = CARTESIAN_POINT ( 'NONE',  ( -11.13100899292000001, -6.505098555691000151, 12.97861128357999938 ) ) ;
#8776 = AXIS2_PLACEMENT_3D ( 'NONE', #3105, #21263, #8550 ) ;
#8777 = CARTESIAN_POINT ( 'NONE',  ( 13.49999999999999467, 9.320410925913344968, -1.763818356871138748 ) ) ;
#8778 = DIRECTION ( 'NONE',  ( 0.7071067811865465735, -0.7071067811865465735, 5.144932599760337753E-08 ) ) ;
#8779 = ORIENTED_EDGE ( 'NONE', *, *, #19913, .T. ) ;
#8780 = DIRECTION ( 'NONE',  ( 1.000000000000000000, 0.000000000000000000, 0.000000000000000000 ) ) ;
#8781 = CARTESIAN_POINT ( 'NONE',  ( 12.52688711657000020, 13.93375672974000068, 0.8660254037843999608 ) ) ;
#8782 = CARTESIAN_POINT ( 'NONE',  ( 22.79406003406850445, -10.10745882294686560, 3.155071022957284477 ) ) ;
#8783 = CARTESIAN_POINT ( 'NONE',  ( -14.00000000000000000, 6.631411874711850452, 6.523104844762785071 ) ) ;
#8784 = CARTESIAN_POINT ( 'NONE',  ( 16.27407148470705067, -0.09565764253358223501, -10.36543647030853421 ) ) ;
#8785 = CARTESIAN_POINT ( 'NONE',  ( -18.98882254156999849, -9.633796120427998488, -5.569900826749999645 ) ) ;
#8786 = ADVANCED_FACE ( 'NONE', ( #18230 ), #6655, .F. ) ;
#8787 = CARTESIAN_POINT ( 'NONE',  ( -1.795619090332999823, 30.15525342005999576, -1.250754954668999996 ) ) ;
#8788 = CONICAL_SURFACE ( 'NONE', #13391, 7.249999994833000727, 0.7853981633972997312 ) ;
#8790 = CONICAL_SURFACE ( 'NONE', #11871, 9.161549281532000322, 0.02565634000431304615 ) ;
#8789 = CARTESIAN_POINT ( 'NONE',  ( -14.74233120679999942, -7.235896531433999357, -6.477854240395999774 ) ) ;
#8791 = CARTESIAN_POINT ( 'NONE',  ( 1.636241036409593397, 29.89441029013897122, -1.410665930300490478 ) ) ;
#8792 = VERTEX_POINT ( 'NONE', #12034 ) ;
#8793 = CARTESIAN_POINT ( 'NONE',  ( 23.28665037521170333, 1.211924610667231450, 9.267172416750026898 ) ) ;
#8794 = CARTESIAN_POINT ( 'NONE',  ( 20.71864993348000183, -2.045817035657000016, 11.22315166757000071 ) ) ;
#8795 = CARTESIAN_POINT ( 'NONE',  ( 24.29989622817865325, 4.963438857751468092, 9.392559902825308171 ) ) ;
#8796 = AXIS2_PLACEMENT_3D ( 'NONE', #16585, #3878, #11271 ) ;
#8797 = DIRECTION ( 'NONE',  ( 1.000000000000000000, 0.000000000000000000, 0.000000000000000000 ) ) ;
#8798 = ORIENTED_EDGE ( 'NONE', *, *, #14150, .T. ) ;
#8799 = DIRECTION ( 'NONE',  ( 0.5000000000000169864, 0.000000000000000000, -0.8660254037844289376 ) ) ;
#8800 = CARTESIAN_POINT ( 'NONE',  ( 5.005054721376160032, 14.15887057945242411, -3.894303575199400846 ) ) ;
#8801 = EDGE_CURVE ( 'NONE', #15589, #2559, #14876, .T. ) ;
#8802 = CARTESIAN_POINT ( 'NONE',  ( 2.434537302296001737, 11.69769071316999920, -4.313724188359998379 ) ) ;
#8803 = EDGE_LOOP ( 'NONE', ( #18470, #5170, #23576, #1404 ) ) ;
#8804 = CARTESIAN_POINT ( 'NONE',  ( 16.32825125730999716, -0.8629760640228999469, 9.162002845358001579 ) ) ;
#8805 = VERTEX_POINT ( 'NONE', #14205 ) ;
#8806 = CIRCLE ( 'NONE', #11888, 11.50000000000000000 ) ;
#8807 = CARTESIAN_POINT ( 'NONE',  ( 0.7852232940904583236, 27.07644705024190657, 2.043071344251131460 ) ) ;
#8808 = CONTEXT_DEPENDENT_SHAPE_REPRESENTATION ( #1544, #15378 ) ;
#8809 = ADVANCED_FACE ( 'NONE', ( #6575, #17603 ), #13958, .T. ) ;
#8810 = CARTESIAN_POINT ( 'NONE',  ( -12.25000000000000000, 1.374666032043000015E-14, 0.000000000000000000 ) ) ;
#8811 = B_SPLINE_SURFACE_WITH_KNOTS ( 'NONE', 3, 3, ( 
 ( #13974, #21251, #4784, #23289, #14094, #21489, #3093, #10479, #19801, #21616, #12167, #23539, #4904, #3212, #23408, #12290, #5032, #10711, #16014, #17864, #19432, #8650, #6825, #17981, #1263, #8775, #6952, #14343, #885, #8288, #21734, #5147, #2842, #12527, #4663 ),
 ( #19916, #3561, #18221, #1622, #7069, #3450, #20153, #23890, #1740, #12868, #20268, #12984, #14794, #16381, #16730, #9010, #20387, #16620, #23773, #7413, #3913, #9244, #9125, #12644, #1853, #30, #22190, #10835, #7175, #9357, #5604, #14569, #21961, #20033, #16499 ),
 ( #12763, #3792, #7295, #22080, #14453, #14688, #7532, #5488, #3672, #18103, #21847, #10944, #11183, #8900, #18569, #11061, #22307, #5375, #1973, #5723, #18331, #18446, #140, #13109, #14912, #20506, #1508, #16267, #23659, #5260, #15712, #22658, #11988, #7898, #2204 ),
 ( #10286, #949, #13913, #16980, #20735, #22431, #8473, #6067, #23102, #9595, #4142, #14037, #2326, #9476, #12109, #18918, #9717, #383, #496, #7780, #17099, #23229, #15266, #17676, #15035, #15148, #19496, #5839, #13337, #11539, #13224, #2905, #2782, #21431, #2086 ) ),
 .UNSPECIFIED., .F., .F., .F.,
 ( 4, 4 ),
 ( 4, 1, 1, 1, 1, 1, 1, 1, 1, 1, 1, 1, 1, 1, 1, 1, 1, 1, 1, 1, 1, 1, 1, 1, 1, 1, 1, 1, 1, 1, 1, 1, 4 ),
 ( -0.1279891693871000047, 1.127989169386999890 ),
 ( -0.02000000000000000042, 0.01250000000000000069, 0.04499999999999999833, 0.07749999999999999944, 0.1100000000000000006, 0.1424999999999999878, 0.1749999999999999889, 0.2074999999999999900, 0.2399999999999999911, 0.2725000000000000200, 0.3049999999999999933, 0.3375000000000000222, 0.3699999999999999956, 0.4025000000000000244, 0.4349999999999999978, 0.4675000000000000266, 0.5000000000000000000, 0.5324999999999999734, 0.5649999999999999467, 0.5975000000000000311, 0.6300000000000000044, 0.6624999999999999778, 0.6949999999999999512, 0.7275000000000000355, 0.7600000000000000089, 0.7924999999999999822, 0.8249999999999999556, 0.8575000000000000400, 0.8900000000000000133, 0.9224999999999999867, 0.9549999999999999600, 0.9875000000000000444, 1.020000000000000018 ),
 .UNSPECIFIED. ) ;
#8812 = VERTEX_POINT ( 'NONE', #10209 ) ;
#8813 = CIRCLE ( 'NONE', #14213, 9.574826156038998448 ) ;
#8814 = B_SPLINE_CURVE_WITH_KNOTS ( 'NONE', 3,
 ( #7847, #22378, #15214, #16924, #22849, #2639, #444, #20807, #13405, #14981 ),
 .UNSPECIFIED., .F., .F.,
 ( 4, 1, 1, 2, 2, 4 ),
 ( 0.000000000000000000, 0.2500000000000011657, 0.3750000000000013323, 0.4375000000000017208, 0.5000000000000019984, 1.000000000000000000 ),
 .UNSPECIFIED. ) ;
#8815 = CARTESIAN_POINT ( 'NONE',  ( -6.637070260807000466, 26.35799170939839797, 1.000000000000000000 ) ) ;
#8816 = CARTESIAN_POINT ( 'NONE',  ( -4.086025793108967186, 15.03144785070672995, -4.562901506959450515 ) ) ;
#8817 = CARTESIAN_POINT ( 'NONE',  ( -23.15201940902000288, -1.306677278990999946, -10.07836265387000019 ) ) ;
#8818 = EDGE_CURVE ( 'NONE', #16646, #13895, #3310, .T. ) ;
#8819 = CARTESIAN_POINT ( 'NONE',  ( -20.02703166550000091, -7.955150927529998306, -5.824612496301999620 ) ) ;
#8820 = CARTESIAN_POINT ( 'NONE',  ( 18.94166666666666288, 4.611704135636504276, -8.001627034636081603 ) ) ;
#8821 = EDGE_CURVE ( 'NONE', #2324, #2392, #3197, .T. ) ;
#8822 = CARTESIAN_POINT ( 'NONE',  ( -23.59826610954376491, 2.101365615520589536, 10.37455059532381263 ) ) ;
#8823 = CARTESIAN_POINT ( 'NONE',  ( 1.475904072323096727, 26.71091357114880083, -1.643089912458857826 ) ) ;
#8824 = CARTESIAN_POINT ( 'NONE',  ( -14.25699038479000080, 13.93375672974000068, 0.000000000000000000 ) ) ;
#8825 = CARTESIAN_POINT ( 'NONE',  ( 1.739122139606305906, 30.68463495477586989, -1.280904342922043693 ) ) ;
#8826 = VERTEX_POINT ( 'NONE', #21107 ) ;
#8827 = CARTESIAN_POINT ( 'NONE',  ( 12.00000000000000000, 0.000000000000000000, -7.500000000002917666 ) ) ;
#8828 = CARTESIAN_POINT ( 'NONE',  ( -1.723852419406000092, 26.85369850837999905, -1.472309056329999866 ) ) ;
#8829 = CONICAL_SURFACE ( 'NONE', #15765, 2.949999959913000236, 0.7853981633972997312 ) ;
#8830 = VECTOR ( 'NONE', #1265, 1000.000000000000000 ) ;
#8831 = CARTESIAN_POINT ( 'NONE',  ( 5.220711627940157307, 14.63818902522256771, -3.265501637091204223 ) ) ;
#8832 = CARTESIAN_POINT ( 'NONE',  ( 1.848781781241999989, 25.77271896306000443, 0.9420013681046000009 ) ) ;
#8833 = EDGE_CURVE ( 'NONE', #7342, #16380, #20677, .T. ) ;
#8834 = CARTESIAN_POINT ( 'NONE',  ( -3.861639638596443547, 12.10487486993750927, 2.911362801195074290 ) ) ;
#8835 = ORIENTED_EDGE ( 'NONE', *, *, #20921, .F. ) ;
#8836 = DIRECTION ( 'NONE',  ( 0.000000000000000000, 0.000000000000000000, -1.000000000000000000 ) ) ;
#8837 = CARTESIAN_POINT ( 'NONE',  ( 4.718949164482028280, 12.40033812480790232, -1.110935410325604833 ) ) ;
#8838 = DIRECTION ( 'NONE',  ( 0.000000000000000000, -1.000000000000000000, 0.000000000000000000 ) ) ;
#8839 = CARTESIAN_POINT ( 'NONE',  ( 1.750000000000000000, 7.000000000000000000, 0.000000000000000000 ) ) ;
#8840 = ORIENTED_EDGE ( 'NONE', *, *, #10886, .F. ) ;
#8841 = CARTESIAN_POINT ( 'NONE',  ( -2.153985071724999756, 30.83999999999999986, 0.1610847937796999751 ) ) ;
#8842 = DIRECTION ( 'NONE',  ( 1.000000000000000000, 0.000000000000000000, 0.000000000000000000 ) ) ;
#8843 = CARTESIAN_POINT ( 'NONE',  ( 17.67093892131000032, 6.655236401869999874, -7.121176743063999837 ) ) ;
#8844 = CARTESIAN_POINT ( 'NONE',  ( 18.70683015900163326, 8.814939528305005823, 5.571978707274588771 ) ) ;
#8845 = VERTEX_POINT ( 'NONE', #17350 ) ;
#8846 = CARTESIAN_POINT ( 'NONE',  ( -1.259047450927251566, 28.66666666666666430, -2.184465970885643316 ) ) ;
#8847 = CARTESIAN_POINT ( 'NONE',  ( -0.9541616508540999853, 30.90409830547999803, -2.061978857876999971 ) ) ;
#8848 = CARTESIAN_POINT ( 'NONE',  ( -12.48665389351999977, 6.877253802972000507, -5.798544038930000255 ) ) ;
#8849 = CARTESIAN_POINT ( 'NONE',  ( 2.500000000000000000, 30.00000000000000000, 0.000000000000000000 ) ) ;
#8850 = ORIENTED_EDGE ( 'NONE', *, *, #13375, .F. ) ;
#8852 = AXIS2_PLACEMENT_3D ( 'NONE', #23028, #624, #19290 ) ;
#8851 = CARTESIAN_POINT ( 'NONE',  ( -14.25699038479000080, -13.93375672974000068, 0.000000000000000000 ) ) ;
#8853 = CARTESIAN_POINT ( 'NONE',  ( -24.33938584177814946, -12.23286334200125758, 3.811912743550009974 ) ) ;
#8854 = DIRECTION ( 'NONE',  ( 1.000000000000000000, 0.000000000000000000, 0.000000000000000000 ) ) ;
#8855 = CARTESIAN_POINT ( 'NONE',  ( 0.5294722038327828173, 24.50879627117540238, -2.335604389998253261 ) ) ;
#8856 = PLANE ( 'NONE',  #16191 ) ;
#8857 = CARTESIAN_POINT ( 'NONE',  ( -3.958969230662715333, 13.89523177694561973, 4.848950307086769662 ) ) ;
#8858 = VECTOR ( 'NONE', #289, 1000.000000000000000 ) ;
#8859 = CARTESIAN_POINT ( 'NONE',  ( -12.25000000000000000, 8.148273666119854042, -12.70947166610607937 ) ) ;
#8860 = CARTESIAN_POINT ( 'NONE',  ( 19.71724770046332154, 7.338844409646621436, 5.639768430530357257 ) ) ;
#8861 = ORIENTED_EDGE ( 'NONE', *, *, #4172, .F. ) ;
#8862 = ADVANCED_FACE ( 'NONE', ( #17852 ), #23274, .F. ) ;
#8863 = DIRECTION ( 'NONE',  ( 0.000000000000000000, 1.000000000000000000, 0.000000000000000000 ) ) ;
#8864 = CARTESIAN_POINT ( 'NONE',  ( 1.350644574821315613, 24.52555747447237877, -3.839035148326051861 ) ) ;
#8865 = AXIS2_PLACEMENT_3D ( 'NONE', #2020, #3841, #5648 ) ;
#8866 = ORIENTED_EDGE ( 'NONE', *, *, #19783, .F. ) ;
#8867 = CARTESIAN_POINT ( 'NONE',  ( 5.983385025969996995, 14.53214776857002022, 1.355298851139999483 ) ) ;
#8868 = CARTESIAN_POINT ( 'NONE',  ( 4.814391914611523937, 13.57103066341566766, 4.918137562955356756 ) ) ;
#8869 = CARTESIAN_POINT ( 'NONE',  ( 6.243179582884000212, 13.63342035941999875, -1.952365010387999922 ) ) ;
#8870 = CARTESIAN_POINT ( 'NONE',  ( -2.500000000000000000, 28.00000000000000000, 0.000000000000000000 ) ) ;
#8871 = VERTEX_POINT ( 'NONE', #4769 ) ;
#8872 = CARTESIAN_POINT ( 'NONE',  ( -2.649085689637681540, 29.97444252552741872, -3.089351817498231068 ) ) ;
#8873 = STYLED_ITEM ( 'NONE', ( #13560 ), #17244 ) ;
#8874 = LINE ( 'NONE', #10568, #8619 ) ;
#8875 = CARTESIAN_POINT ( 'NONE',  ( 1.699999999999999956, 9.000014497636620092, -0.2828405775381332421 ) ) ;
#8876 = VERTEX_POINT ( 'NONE', #2950 ) ;
#8877 = CLOSED_SHELL ( 'NONE', ( #10670, #12078, #4942, #17211, #2113 ) ) ;
#8878 = CARTESIAN_POINT ( 'NONE',  ( -21.29002284374999832, -1.712745750557999935, 10.57005027581000078 ) ) ;
#8879 = FACE_OUTER_BOUND ( 'NONE', #7462, .T. ) ;
#8880 = CARTESIAN_POINT ( 'NONE',  ( 14.55000962749105931, 3.050471366525244310, -9.861052313355841648 ) ) ;
#8881 = AXIS2_PLACEMENT_3D ( 'NONE', #14176, #23248, #10305 ) ;
#8882 = CARTESIAN_POINT ( 'NONE',  ( 23.53832649037999758, 6.487047738608999303, -9.238512469485000267 ) ) ;
#8883 = CARTESIAN_POINT ( 'NONE',  ( 0.2266750768320999754, 29.07716145795999907, -2.156108152400999955 ) ) ;
#8884 = CARTESIAN_POINT ( 'NONE',  ( -24.00016455340000121, 1.715543117993999783E-14, 0.000000000000000000 ) ) ;
#8885 = CARTESIAN_POINT ( 'NONE',  ( -3.150245644565998759, 12.00172895669998674, -3.533903776844997235 ) ) ;
#8886 = ORIENTED_EDGE ( 'NONE', *, *, #17835, .T. ) ;
#8887 = CARTESIAN_POINT ( 'NONE',  ( -21.50592920454664636, 8.059125700889071098, -4.644844294440694021 ) ) ;
#8888 = AXIS2_PLACEMENT_3D ( 'NONE', #19132, #11879, #23247 ) ;
#8889 = ORIENTED_EDGE ( 'NONE', *, *, #20932, .F. ) ;
#8890 = CARTESIAN_POINT ( 'NONE',  ( -1.999167105995452998, 29.51666666666667282, -1.536366799937284089 ) ) ;
#8891 = CARTESIAN_POINT ( 'NONE',  ( 24.50000000000000000, -9.958777891625446799, 3.453140405739827390 ) ) ;
#8892 = CONICAL_SURFACE ( 'NONE', #23957, 2.197442471388999952, 0.7853981633972997312 ) ;
#8893 = CONICAL_SURFACE ( 'NONE', #7713, 9.630770167580999797, 0.9419447502231289571 ) ;
#8894 = ORIENTED_EDGE ( 'NONE', *, *, #3881, .F. ) ;
#8895 = CARTESIAN_POINT ( 'NONE',  ( 17.42999999999999972, 9.118569865760999704, 0.000000000000000000 ) ) ;
#8896 = FACE_OUTER_BOUND ( 'NONE', #23436, .T. ) ;
#8897 = CARTESIAN_POINT ( 'NONE',  ( 13.24950470672999892, -0.4381588468272000214, 10.97213491105999950 ) ) ;
#8898 = ADVANCED_FACE ( 'NONE', ( #10337 ), #13318, .T. ) ;
#8899 = VERTEX_POINT ( 'NONE', #1127 ) ;
#8900 = CARTESIAN_POINT ( 'NONE',  ( -10.30168113877000025, 9.808725055038999940, 11.63569968352999950 ) ) ;
#8901 = CARTESIAN_POINT ( 'NONE',  ( 13.50000000000000000, 7.993555678485630089, -4.730236700590047860 ) ) ;
#8902 = CARTESIAN_POINT ( 'NONE',  ( -14.29262082160975567, -13.66753291840124085, -1.327138571210202400 ) ) ;
#8903 = AXIS2_PLACEMENT_3D ( 'NONE', #4131, #20608, #2191 ) ;
#8904 = VERTEX_POINT ( 'NONE', #1613 ) ;
#8905 = CARTESIAN_POINT ( 'NONE',  ( 20.94094110115653962, -9.546404809872933939, 4.471938574268008892 ) ) ;
#8906 = CARTESIAN_POINT ( 'NONE',  ( -14.00000000000000355, 2.181633025534562176, 9.406358577098494322 ) ) ;
#8907 = CARTESIAN_POINT ( 'NONE',  ( 17.01556895440440798, 5.718620203982503369, 8.698992263909991252 ) ) ;
#8908 = CARTESIAN_POINT ( 'NONE',  ( 2.142501703538999713, 30.65881256477999983, -0.4453337693464999858 ) ) ;
#8909 = CIRCLE ( 'NONE', #19751, 3.000000000000000000 ) ;
#8910 = PRODUCT_DEFINITION_CONTEXT ( 'detailed design', #23342, 'design' ) ;
#8911 = CARTESIAN_POINT ( 'NONE',  ( -12.37247714714999880, 8.083715232074000667, -4.229267010826999851 ) ) ;
#8912 = CARTESIAN_POINT ( 'NONE',  ( 1.882286714434961761, 29.86920771456559365, -1.059984207813917445 ) ) ;
#8913 = ORIENTED_EDGE ( 'NONE', *, *, #16750, .T. ) ;
#8914 = CARTESIAN_POINT ( 'NONE',  ( -24.27585716845300112, -3.329860787244067311, 12.49993117327242587 ) ) ;
#8915 = CARTESIAN_POINT ( 'NONE',  ( 22.45790833551999910, 0.8992737871539999706, 11.42083163704999826 ) ) ;
#8916 = CARTESIAN_POINT ( 'NONE',  ( 22.17189245347322313, 10.72406570084320698, -0.06313349674599283423 ) ) ;
#8917 = CARTESIAN_POINT ( 'NONE',  ( -0.8595773952324387013, 23.63862887798046586, -1.958280311448067579 ) ) ;
#8918 = EDGE_LOOP ( 'NONE', ( #19549, #17173, #23538, #3361, #21492 ) ) ;
#8919 = LINE ( 'NONE', #1405, #14918 ) ;
#8920 = DIRECTION ( 'NONE',  ( 0.000000000000000000, 1.000000000000000000, 0.000000000000000000 ) ) ;
#8921 = CARTESIAN_POINT ( 'NONE',  ( 3.772394398227998380, 12.11624026657999131, -2.973371410456998376 ) ) ;
#8922 = ORIENTED_EDGE ( 'NONE', *, *, #7730, .T. ) ;
#8923 = EDGE_CURVE ( 'NONE', #3365, #20695, #11843, .T. ) ;
#8924 = CARTESIAN_POINT ( 'NONE',  ( 12.52688711657000020, -6.216878364870000340, -12.50000000000000000 ) ) ;
#8925 = ORIENTED_EDGE ( 'NONE', *, *, #3091, .F. ) ;
#8926 = CARTESIAN_POINT ( 'NONE',  ( -1.834421572440270376, 26.90385776341792834, 1.215053711552148696 ) ) ;
#8927 = CARTESIAN_POINT ( 'NONE',  ( 2.500000000000001776, 29.98333333333333783, 0.3272492347489265874 ) ) ;
#8928 = ORIENTED_EDGE ( 'NONE', *, *, #22063, .T. ) ;
#8929 = DIRECTION ( 'NONE',  ( 0.000000000000000000, 1.000000000000000000, 0.000000000000000000 ) ) ;
#8930 = CARTESIAN_POINT ( 'NONE',  ( -23.79436614888999912, -7.215319973546000298, 7.181436178667000902 ) ) ;
#8931 = ADVANCED_FACE ( 'NONE', ( #23526 ), #16812, .T. ) ;
#8932 = CARTESIAN_POINT ( 'NONE',  ( -15.55816401016000050, 8.955035067704001150, 3.817101925073999702 ) ) ;
#8933 = CARTESIAN_POINT ( 'NONE',  ( 18.60154166666664821, -5.622352741887121752, -7.315769444643206221 ) ) ;
#8934 = CARTESIAN_POINT ( 'NONE',  ( -24.16443887599344365, 8.804325591011858521, -5.901198901063593460 ) ) ;
#8935 = CARTESIAN_POINT ( 'NONE',  ( 0.7772763509246626290, 27.55895043119048182, -2.062997027023658614 ) ) ;
#8936 = CARTESIAN_POINT ( 'NONE',  ( -5.774423697881004180, 15.72625884058998302, 1.905284384892999228 ) ) ;
#8937 = CARTESIAN_POINT ( 'NONE',  ( 2.146814458760614386, 30.61776554068781309, -0.2373564554389892833 ) ) ;
#8938 = VERTEX_POINT ( 'NONE', #5475 ) ;
#8939 = CARTESIAN_POINT ( 'NONE',  ( 23.19213215653367044, 9.263419914609070105, 1.127708713065163293 ) ) ;
#8940 = CARTESIAN_POINT ( 'NONE',  ( 1.429826439988904019, 26.29738147351989141, 1.686326896136374653 ) ) ;
#8941 = CARTESIAN_POINT ( 'NONE',  ( 0.1453149127350999992, 27.64163313894999874, -2.464088664829000130 ) ) ;
#8942 = EDGE_CURVE ( 'NONE', #1386, #4476, #18430, .T. ) ;
#8943 = CARTESIAN_POINT ( 'NONE',  ( 5.925978167137946784, 14.42557216884380900, -1.550677319624406580 ) ) ;
#8944 = CARTESIAN_POINT ( 'NONE',  ( 1.617729300723999897, 27.33271896306000315, 1.617729300723999897 ) ) ;
#8945 = AXIS2_PLACEMENT_3D ( 'NONE', #21053, #23098, #11855 ) ;
#8946 = CARTESIAN_POINT ( 'NONE',  ( 4.418282465362906919, 12.29075935838933020, 1.985689274626368572 ) ) ;
#8947 = ORIENTED_EDGE ( 'NONE', *, *, #15869, .T. ) ;
#8948 = CARTESIAN_POINT ( 'NONE',  ( 17.69454166666665529, 5.608048916488373337, 7.297156872939496886 ) ) ;
#8949 = EDGE_CURVE ( 'NONE', #6003, #2681, #1739, .T. ) ;
#8950 = CARTESIAN_POINT ( 'NONE',  ( 4.761208897123116124, 12.41619411356198555, -0.9207184844910151211 ) ) ;
#8951 = CARTESIAN_POINT ( 'NONE',  ( -10.58070998671075280, 15.47950041580538638, 1.445153319346881959 ) ) ;
#8952 = CARTESIAN_POINT ( 'NONE',  ( -2.147911019905105690, 30.79742692913817592, -0.5598789276575362184 ) ) ;
#8953 = ORIENTED_EDGE ( 'NONE', *, *, #190, .T. ) ;
#8954 = CARTESIAN_POINT ( 'NONE',  ( 1.259047450927277323, 24.26666666666667282, 2.184465970885627772 ) ) ;
#8955 = CARTESIAN_POINT ( 'NONE',  ( -15.95055420454664841, 9.080604370815557047, -1.188521384907452294 ) ) ;
#8956 = CARTESIAN_POINT ( 'NONE',  ( 18.00000142131000302, 9.258615172493000145, 3.074095935696000037 ) ) ;
#8957 = CARTESIAN_POINT ( 'NONE',  ( 18.82474110796517053, 5.884666067428870662, 8.614044124011082104 ) ) ;
#8958 = EDGE_CURVE ( 'NONE', #14317, #568, #6374, .T. ) ;
#8959 = CARTESIAN_POINT ( 'NONE',  ( -24.50000000000000000, 2.324045842668999493E-14, 12.50000000000000000 ) ) ;
#8960 = CARTESIAN_POINT ( 'NONE',  ( 2.033768963815000053, 28.90151168796999670, 0.6996504102948000181 ) ) ;
#8961 = CARTESIAN_POINT ( 'NONE',  ( -9.000000000000000000, 18.50000000000000000, -6.000000000000000000 ) ) ;
#8962 = CARTESIAN_POINT ( 'NONE',  ( 13.50000000000000355, -8.015790134246481458, 6.051666939700164782 ) ) ;
#8963 = ORIENTED_EDGE ( 'NONE', *, *, #2422, .T. ) ;
#8964 = DIRECTION ( 'NONE',  ( 0.000000000000000000, -1.000000000000000000, 0.000000000000000000 ) ) ;
#8965 = CARTESIAN_POINT ( 'NONE',  ( 24.29098604190999922, 10.32447825566000077, 3.305036642305999806 ) ) ;
#8966 = PLANE ( 'NONE',  #5407 ) ;
#8967 = FACE_OUTER_BOUND ( 'NONE', #968, .T. ) ;
#8968 = DIRECTION ( 'NONE',  ( 0.000000000000000000, 0.000000000000000000, 1.000000000000000000 ) ) ;
#8969 = CARTESIAN_POINT ( 'NONE',  ( 3.419138964049998286, 12.01219122919000526, 3.585892243584002159 ) ) ;
#8970 = CARTESIAN_POINT ( 'NONE',  ( -12.24999999999999822, 10.32537944888909642, -10.67953724782443814 ) ) ;
#8971 = EDGE_LOOP ( 'NONE', ( #633, #19527, #17579, #8866 ) ) ;
#8972 = CARTESIAN_POINT ( 'NONE',  ( 0.000000000000000000, 17.95000004008999994, 0.000000000000000000 ) ) ;
#8973 = CARTESIAN_POINT ( 'NONE',  ( -4.000000000000000000, 26.37490599056222962, 1.464369514602714251 ) ) ;
#8974 = ORIENTED_EDGE ( 'NONE', *, *, #10021, .T. ) ;
#8975 = CARTESIAN_POINT ( 'NONE',  ( -1.937279285829999864, 24.60217777461999944, 0.9581223917076999719 ) ) ;
#8976 = EDGE_CURVE ( 'NONE', #20510, #21669, #5134, .T. ) ;
#8977 = DIRECTION ( 'NONE',  ( 0.000000000000000000, 1.000000000000000000, 0.000000000000000000 ) ) ;
#8978 = CARTESIAN_POINT ( 'NONE',  ( 11.18574820343433807, -1.750427062344837914, -12.50001947253043078 ) ) ;
#8979 = ADVANCED_FACE ( 'NONE', ( #9227 ), #1840, .F. ) ;
#8980 = DIRECTION ( 'NONE',  ( 1.000000000000000000, 0.000000000000000000, 0.000000000000000000 ) ) ;
#8981 = CARTESIAN_POINT ( 'NONE',  ( -5.942997347608004688, 15.81517321836000178, -1.152667559718999923 ) ) ;
#8982 = CIRCLE ( 'NONE', #6646, 5.625000000000000000 ) ;
#8983 = CARTESIAN_POINT ( 'NONE',  ( 0.000000000000000000, 0.000000000000000000, 0.000000000000000000 ) ) ;
#8984 = VERTEX_POINT ( 'NONE', #19901 ) ;
#8985 = CARTESIAN_POINT ( 'NONE',  ( -14.74233120679999942, -7.235896531433999357, -6.477854240395999774 ) ) ;
#8986 = FACE_OUTER_BOUND ( 'NONE', #9094, .T. ) ;
#8987 = CARTESIAN_POINT ( 'NONE',  ( -3.999987874060712656, 24.60222989788993431, 1.328900689436825377 ) ) ;
#8988 = ORIENTED_EDGE ( 'NONE', *, *, #17552, .T. ) ;
#8989 = EDGE_CURVE ( 'NONE', #23711, #2468, #11748, .T. ) ;
#8990 = CARTESIAN_POINT ( 'NONE',  ( -10.82553598051486787, 15.36695194536291353, -1.671868630953385004 ) ) ;
#8991 = CARTESIAN_POINT ( 'NONE',  ( 1.487333709577000063, 24.19292139875000203, -1.545051636020000174 ) ) ;
#8992 = CARTESIAN_POINT ( 'NONE',  ( 14.67988943935569957, 7.031391890844531645, -7.575081847691048864 ) ) ;
#8993 = CIRCLE ( 'NONE', #20278, 1.000000000000000000 ) ;
#8994 = FACE_OUTER_BOUND ( 'NONE', #18319, .T. ) ;
#8995 = CARTESIAN_POINT ( 'NONE',  ( 21.51930989774999858, -1.098377462729000165, -11.17932485002999954 ) ) ;
#8996 = CARTESIAN_POINT ( 'NONE',  ( -0.6988337043581999142, 30.62333119616999966, -2.254725353931999798 ) ) ;
#8997 = CARTESIAN_POINT ( 'NONE',  ( 13.79014734960547450, 9.020246190001508069, -0.3553286354086955812 ) ) ;
#8998 = CARTESIAN_POINT ( 'NONE',  ( -4.363055774502002215, 12.47547100499999395, -2.048634389234999631 ) ) ;
#8999 = B_SPLINE_CURVE_WITH_KNOTS ( 'NONE', 3,
 ( #15336, #2636, #2387, #9778, #13528, #10031, #15577, #21166, #13764, #4577, #11968, #19357, #9542, #13206, #14898, #1839, #22289, #16836 ),
 .UNSPECIFIED., .F., .F.,
 ( 4, 2, 2, 2, 2, 2, 2, 2, 4 ),
 ( 0.000000000000000000, 0.1250000000000000000, 0.2500000000000000000, 0.3750000000000000000, 0.5000000000000000000, 0.6250000000000000000, 0.7500000000000000000, 0.8750000000000000000, 1.000000000000000000 ),
 .UNSPECIFIED. ) ;
#9000 = DIRECTION ( 'NONE',  ( 1.000000000000000000, 0.000000000000000000, 0.000000000000000000 ) ) ;
#9001 = ORIENTED_EDGE ( 'NONE', *, *, #12487, .F. ) ;
#9002 = VECTOR ( 'NONE', #4877, 1000.000000000000000 ) ;
#9003 = CARTESIAN_POINT ( 'NONE',  ( 24.50000000000000000, -8.246372141814999779, 6.625187740483999832 ) ) ;
#9004 = EDGE_LOOP ( 'NONE', ( #2318, #399, #21121, #3175 ) ) ;
#9005 = CARTESIAN_POINT ( 'NONE',  ( -1.853875633792771760, 30.49394709125570557, 1.681730189323883629 ) ) ;
#9006 = CARTESIAN_POINT ( 'NONE',  ( 16.52299999999999969, -9.095294458157999529, 0.000000000000000000 ) ) ;
#9007 = CARTESIAN_POINT ( 'NONE',  ( 18.75008227645999881, -9.152445778720998959, 0.000000000000000000 ) ) ;
#9008 = CARTESIAN_POINT ( 'NONE',  ( 16.64424246484000136, 10.59610064161999965, 3.219381317545000343 ) ) ;
#9009 = ORIENTED_EDGE ( 'NONE', *, *, #12093, .T. ) ;
#9010 = CARTESIAN_POINT ( 'NONE',  ( -10.30905506584999998, 14.86577284560999956, 0.2581334465446999960 ) ) ;
#9011 = CARTESIAN_POINT ( 'NONE',  ( 13.50000000000000000, 8.034926714834112360, -4.667990898080017992 ) ) ;
#9012 = CARTESIAN_POINT ( 'NONE',  ( 0.000000000000000000, 15.09999999999999964, 0.000000000000000000 ) ) ;
#9013 = VERTEX_POINT ( 'NONE', #12631 ) ;
#9014 = FACE_OUTER_BOUND ( 'NONE', #4383, .T. ) ;
#9015 = CARTESIAN_POINT ( 'NONE',  ( 21.67630575707568852, 5.728324180010714528, -9.603614269126266478 ) ) ;
#9016 = AXIS2_PLACEMENT_3D ( 'NONE', #746, #1116, #17220 ) ;
#9017 = CARTESIAN_POINT ( 'NONE',  ( -14.25243324638999809, -13.93375672974000068, 0.8660254037843999608 ) ) ;
#9018 = CARTESIAN_POINT ( 'NONE',  ( 16.10201719184190949, -5.936034372256892233, -8.493431826325096523 ) ) ;
#9019 = CARTESIAN_POINT ( 'NONE',  ( -18.60187077250666832, -5.622357932043938078, 7.315776198232815553 ) ) ;
#9020 = CARTESIAN_POINT ( 'NONE',  ( -14.45529013989012057, -12.11766535962171965, 4.011530336787306084 ) ) ;
#9021 = CARTESIAN_POINT ( 'NONE',  ( -12.91415807507000046, -6.873022849445000304, -6.789234046460999927 ) ) ;
#9022 = CARTESIAN_POINT ( 'NONE',  ( 2.133167008818035004, 29.82381322641220578, -0.3387237046597101897 ) ) ;
#9023 = ORIENTED_EDGE ( 'NONE', *, *, #23758, .T. ) ;
#9024 = CARTESIAN_POINT ( 'NONE',  ( -23.74465998031000069, -6.216878364870000340, 12.50000000000000000 ) ) ;
#9025 = CARTESIAN_POINT ( 'NONE',  ( 21.54767801288958395, -5.974488166519072330, -8.885303408042284801 ) ) ;
#9026 = CARTESIAN_POINT ( 'NONE',  ( 0.000000000000000000, 26.50000000000000355, 0.000000000000000000 ) ) ;
#9027 = ORIENTED_EDGE ( 'NONE', *, *, #1252, .T. ) ;
#9028 = DIRECTION ( 'NONE',  ( 0.5000000000000169864, -0.8660254037844289376, 0.000000000000000000 ) ) ;
#9029 = CARTESIAN_POINT ( 'NONE',  ( 4.830315656668564550, 14.72903184301115687, -3.766121966294526668 ) ) ;
#9030 = AXIS2_PLACEMENT_3D ( 'NONE', #3125, #21153, #15811 ) ;
#9031 = B_SPLINE_CURVE_WITH_KNOTS ( 'NONE', 3,
 ( #4528, #16009, #11919, #6585, #2838, #1377, #4657, #23284, #8770, #4778, #21611, #1139, #8535, #15893, #17486, #2716, #12285, #16133, #12162, #19675, #6697, #6821, #14089, #3087, #880, #12043, #6336, #10348, #5028, #19427, #10218, #14214, #23165, #13970, #17736, #10474, #17860, #8645, #23404, #12412, #19796, #13719, #1504, #20378, #5482, #20028 ),
 .UNSPECIFIED., .F., .F.,
 ( 4, 1, 1, 1, 2, 2, 1, 1, 1, 1, 1, 1, 2, 2, 1, 1, 1, 1, 1, 2, 2, 1, 1, 1, 2, 2, 1, 1, 1, 1, 1, 2, 2, 4 ),
 ( 0.000000000000000000, 0.1250000000000003608, 0.1875000000000006661, 0.2187500000000007494, 0.2343750000000008882, 0.2500000000000010547, 0.3750000000000022204, 0.4375000000000028311, 0.4687500000000032196, 0.4843750000000035527, 0.4921875000000037192, 0.4960937500000037748, 0.4980468750000037748, 0.5000000000000037748, 0.5625000000000025535, 0.5937500000000017764, 0.6093750000000015543, 0.6171875000000013323, 0.6210937500000012212, 0.6230468750000011102, 0.6250000000000009992, 0.6875000000000011102, 0.7187500000000012212, 0.7343750000000012212, 0.7421875000000012212, 0.7500000000000012212, 0.8125000000000014433, 0.8437500000000015543, 0.8593750000000015543, 0.8671875000000016653, 0.8710937500000016653, 0.8730468750000015543, 0.8750000000000014433, 1.000000000000000000 ),
 .UNSPECIFIED. ) ;
#9032 = CARTESIAN_POINT ( 'NONE',  ( 4.257195002520998806, 12.20674677251999896, -2.334155036774002490 ) ) ;
#9033 = ORIENTED_EDGE ( 'NONE', *, *, #6076, .T. ) ;
#9034 = CARTESIAN_POINT ( 'NONE',  ( 0.000000000000000000, 26.50000000000000355, 0.000000000000000000 ) ) ;
#9035 = ORIENTED_EDGE ( 'NONE', *, *, #6572, .F. ) ;
#9036 = CARTESIAN_POINT ( 'NONE',  ( -5.319412312564031353, 16.04959412292968324, 3.038395077758344609 ) ) ;
#9037 = SHAPE_DEFINITION_REPRESENTATION ( #18671, #14475 ) ;
#9038 = CARTESIAN_POINT ( 'NONE',  ( 1.536366799937295413, 29.88333333333333641, 1.999167105995444338 ) ) ;
#9039 = ORIENTED_EDGE ( 'NONE', *, *, #18533, .F. ) ;
#9040 = CARTESIAN_POINT ( 'NONE',  ( 2.434987841376199835, 24.43331912268990180, -0.6540909589892343057 ) ) ;
#9041 = CARTESIAN_POINT ( 'NONE',  ( -20.90380581945999694, 9.909073374132001177, -1.964704235543000221 ) ) ;
#9042 = CARTESIAN_POINT ( 'NONE',  ( -16.37068540204000300, -7.269710435383999858, -6.508117440121999664 ) ) ;
#9043 = CARTESIAN_POINT ( 'NONE',  ( -4.080056528100000079, 28.00000000000000000, 4.563746053395999702 ) ) ;
#9044 = CARTESIAN_POINT ( 'NONE',  ( -23.67547148678552560, 4.768064527406466802, 9.453135388948583184 ) ) ;
#9045 = CARTESIAN_POINT ( 'NONE',  ( -1.443311851948678060, 26.31339629256746804, 1.671814658486965088 ) ) ;
#9046 = CARTESIAN_POINT ( 'NONE',  ( -0.3933730402102999513, 28.24250240010000113, 2.844001364980000002 ) ) ;
#9047 = EDGE_CURVE ( 'NONE', #10311, #21798, #14554, .T. ) ;
#9048 = CARTESIAN_POINT ( 'NONE',  ( 1.386897540580403820, 30.71498289799559345, -1.655823646851495967 ) ) ;
#9049 = ORIENTED_EDGE ( 'NONE', *, *, #19755, .F. ) ;
#9050 = CARTESIAN_POINT ( 'NONE',  ( -17.65117920454668266, 8.886717484751601503, 2.388369308413305525 ) ) ;
#9051 = CARTESIAN_POINT ( 'NONE',  ( -24.12232999016000079, 1.520060141252000183E-14, 0.000000000000000000 ) ) ;
#9052 = CARTESIAN_POINT ( 'NONE',  ( 1.640193969998194001, 24.74015355458762144, 1.405240085690787843 ) ) ;
#9053 = MANIFOLD_SOLID_BREP ( 'Stock-MAS-673-1', #10020 ) ;
#9054 = B_SPLINE_CURVE_WITH_KNOTS ( 'NONE', 3,
 ( #19984, #23360, #6540, #1338, #23489, #3282, #10664, #8853, #21566, #6654, #6900, #10786, #23615, #10427 ),
 .UNSPECIFIED., .F., .F.,
 ( 4, 2, 2, 2, 2, 2, 4 ),
 ( 0.000000000000000000, 0.2499999999999999445, 0.3749999999999998890, 0.4999999999999998890, 0.6249999999999998890, 0.7499999999999997780, 1.000000000000000000 ),
 .UNSPECIFIED. ) ;
#9055 = CARTESIAN_POINT ( 'NONE',  ( -0.6185023500890999282, 26.04687716036000111, -2.370125023230000405 ) ) ;
#9056 = CARTESIAN_POINT ( 'NONE',  ( 4.069542469406499663, 12.17106568498275720, 2.629390757502099607 ) ) ;
#9057 = ORIENTED_EDGE ( 'NONE', *, *, #17108, .F. ) ;
#9058 = CARTESIAN_POINT ( 'NONE',  ( -0.9155538765149698888, 11.51860325008744823, -4.724858359221649096 ) ) ;
#9059 = EDGE_CURVE ( 'NONE', #9517, #10732, #10902, .T. ) ;
#9060 = CARTESIAN_POINT ( 'NONE',  ( -11.04281598264000053, 15.31903517167999951, 1.878299281558999834 ) ) ;
#9061 = CARTESIAN_POINT ( 'NONE',  ( -0.9421903349202591649, 29.37597597608807831, 2.074010226627299502 ) ) ;
#9062 = CONICAL_SURFACE ( 'NONE', #1714, 4.309401076758999416, 1.119376321708719590 ) ;
#9063 = ORIENTED_EDGE ( 'NONE', *, *, #11482, .F. ) ;
#9064 = LINE ( 'NONE', #18383, #15389 ) ;
#9065 = CARTESIAN_POINT ( 'NONE',  ( 16.49081408530999937, 8.848325411959001130, 5.124349347825999601 ) ) ;
#9066 = CARTESIAN_POINT ( 'NONE',  ( 18.78241513702097976, 7.121959644642507747, 7.638015814842760598 ) ) ;
#9067 = CARTESIAN_POINT ( 'NONE',  ( -1.999167105995446780, 29.11753006952333322, 1.536366799937292305 ) ) ;
#9068 = CARTESIAN_POINT ( 'NONE',  ( -1.665222063820000153, 29.43094945177000099, 1.361169993929999933 ) ) ;
#9069 = AXIS2_PLACEMENT_3D ( 'NONE', #6854, #14249, #5173 ) ;
#9070 = CARTESIAN_POINT ( 'NONE',  ( -12.47823091122000072, 7.040259760702999969, -5.593011138739999666 ) ) ;
#9071 = CARTESIAN_POINT ( 'NONE',  ( 13.50000000000000355, -9.410104611735745195, -1.703795694468760447 ) ) ;
#9072 = ORIENTED_EDGE ( 'NONE', *, *, #19105, .F. ) ;
#9073 = DIRECTION ( 'NONE',  ( -1.000000000000000000, 0.000000000000000000, 0.000000000000000000 ) ) ;
#9074 = CARTESIAN_POINT ( 'NONE',  ( 23.66558326540000223, 6.907618760750000142, -9.009360667880999429 ) ) ;
#9075 = EDGE_CURVE ( 'NONE', #17995, #22357, #11165, .T. ) ;
#9076 = CARTESIAN_POINT ( 'NONE',  ( -7.034000000000000696, 11.50000000000000000, 2.869609411205000113E-11 ) ) ;
#9077 = CARTESIAN_POINT ( 'NONE',  ( 24.49999999999999645, -7.300324094424125221, 7.693460009872119088 ) ) ;
#9078 = DIRECTION ( 'NONE',  ( 0.000000000000000000, -0.9999999999994555466, 1.043416718096953418E-06 ) ) ;
#9079 = AXIS2_PLACEMENT_3D ( 'NONE', #6599, #12058, #4792 ) ;
#9080 = CARTESIAN_POINT ( 'NONE',  ( -4.823016552992995365, 12.46847780471999734, 1.104821929769999933 ) ) ;
#9081 = CARTESIAN_POINT ( 'NONE',  ( 1.894783946879184722, 29.06763461832910167, -1.038242862623748985 ) ) ;
#9082 = CARTESIAN_POINT ( 'NONE',  ( -22.97909504101000167, -8.290368976810999158, 7.428505582751999903 ) ) ;
#9083 = ORIENTED_EDGE ( 'NONE', *, *, #6748, .T. ) ;
#9084 = CARTESIAN_POINT ( 'NONE',  ( 23.41677564524290744, 34.01856778792605240, 6.000000000000005329 ) ) ;
#9085 = AXIS2_PLACEMENT_3D ( 'NONE', #13738, #8182, #10954 ) ;
#9086 = ORIENTED_EDGE ( 'NONE', *, *, #6581, .F. ) ;
#9087 = CARTESIAN_POINT ( 'NONE',  ( -2.127787408056999841, 23.76613442030999934, 0.3788700132753000105 ) ) ;
#9088 = CARTESIAN_POINT ( 'NONE',  ( 6.027841067254001928, 13.76213909426999038, 1.750693181843999469 ) ) ;
#9089 = ADVANCED_FACE ( 'NONE', ( #16716 ), #23387, .T. ) ;
#9090 = CARTESIAN_POINT ( 'NONE',  ( 11.29022434644176975, -2.380282113944267586, -12.49997383652820560 ) ) ;
#9091 = CARTESIAN_POINT ( 'NONE',  ( 13.21250000000000036, 0.000000000000000000, 0.000000000000000000 ) ) ;
#9092 = CARTESIAN_POINT ( 'NONE',  ( -6.058172502568998752, 16.51671562621000788, -0.9499346773648004172 ) ) ;
#9093 = CARTESIAN_POINT ( 'NONE',  ( 12.54206408531000072, 8.432320343758000547, -5.597842903599000053 ) ) ;
#9094 = EDGE_LOOP ( 'NONE', ( #4243, #14485, #12922, #1161 ) ) ;
#9095 = DIRECTION ( 'NONE',  ( -1.000000000000000000, 0.000000000000000000, 0.000000000000000000 ) ) ;
#9096 = AXIS2_PLACEMENT_3D ( 'NONE', #1456, #18179, #15851 ) ;
#9097 = CARTESIAN_POINT ( 'NONE',  ( -1.973507970679954981, 26.24528935287325737, 0.8411564517195385671 ) ) ;
#9098 = EDGE_CURVE ( 'NONE', #16136, #9967, #11405, .T. ) ;
#9099 = CARTESIAN_POINT ( 'NONE',  ( -23.75856372112281178, -13.93375672973999890, -3.388131789017201356E-17 ) ) ;
#9100 = ORIENTED_EDGE ( 'NONE', *, *, #3558, .F. ) ;
#9101 = DIRECTION ( 'NONE',  ( 1.000000000000000000, 0.000000000000000000, 0.000000000000000000 ) ) ;
#9102 = CARTESIAN_POINT ( 'NONE',  ( 1.634048540053999909, 24.00079805554999979, 1.388967512015999883 ) ) ;
#9103 = CARTESIAN_POINT ( 'NONE',  ( 14.42166414075703784, -1.434770972873324002, -10.21765703208912157 ) ) ;
#9104 = CARTESIAN_POINT ( 'NONE',  ( -2.500000000000000000, 29.03419673619000108, 0.000000000000000000 ) ) ;
#9105 = CARTESIAN_POINT ( 'NONE',  ( 19.64691490199999890, -8.083823404160000337, -7.725524090809999578 ) ) ;
#9106 = ADVANCED_FACE ( 'NONE', ( #22639 ), #7644, .F. ) ;
#9107 = CARTESIAN_POINT ( 'NONE',  ( -1.851011522465999981, 29.22077922916000148, -1.128689685153000166 ) ) ;
#9108 = CARTESIAN_POINT ( 'NONE',  ( 13.73279381853092218, 8.783345170398582979, -2.087887316596209075 ) ) ;
#9109 = EDGE_CURVE ( 'NONE', #1172, #709, #6051, .T. ) ;
#9110 = CARTESIAN_POINT ( 'NONE',  ( -6.046835300290999804, 16.30334124114000360, 1.000000020649999932 ) ) ;
#9111 = PRESENTATION_STYLE_ASSIGNMENT (( #1721 ) ) ;
#9112 = EDGE_LOOP ( 'NONE', ( #13628, #14007, #21873, #22493 ) ) ;
#9113 = AXIS2_PLACEMENT_3D ( 'NONE', #11488, #4213, #18864 ) ;
#9114 = CARTESIAN_POINT ( 'NONE',  ( 24.50000000000000711, -10.15712295534905607, 1.516248268602033100 ) ) ;
#9115 = ORIENTED_EDGE ( 'NONE', *, *, #22555, .T. ) ;
#9116 = DIRECTION ( 'NONE',  ( 0.000000000000000000, 0.7071067811866525998, -0.7071067811864425456 ) ) ;
#9117 = CARTESIAN_POINT ( 'NONE',  ( 17.24104166666665705, 7.287850587087861598, -5.600897003789193640 ) ) ;
#9118 = EDGE_CURVE ( 'NONE', #16168, #3528, #16037, .T. ) ;
#9119 = DIRECTION ( 'NONE',  ( 0.000000000000000000, 0.000000000000000000, -1.000000000000000000 ) ) ;
#9120 = EDGE_CURVE ( 'NONE', #14191, #4710, #13092, .T. ) ;
#9121 = CARTESIAN_POINT ( 'NONE',  ( 17.21942445932999988, -10.43099376775999865, 3.766336729935999994 ) ) ;
#9122 = CARTESIAN_POINT ( 'NONE',  ( -16.28879905794757832, 6.724608735979642482, 7.932750281745096999 ) ) ;
#9123 = CARTESIAN_POINT ( 'NONE',  ( 0.1571687770951999963, 27.27212896666999953, -2.665093312283999705 ) ) ;
#9124 = ORIENTED_EDGE ( 'NONE', *, *, #11153, .F. ) ;
#9125 = CARTESIAN_POINT ( 'NONE',  ( -11.02181256584999858, -14.64514436291000088, -2.564679662907999536 ) ) ;
#9126 = FACE_OUTER_BOUND ( 'NONE', #12153, .T. ) ;
#9127 = CARTESIAN_POINT ( 'NONE',  ( 0.000000000000000000, 28.30000000000000071, -4.618802153517000519 ) ) ;
#9128 = CIRCLE ( 'NONE', #4087, 4.750000000000000000 ) ;
#9129 = ORIENTED_EDGE ( 'NONE', *, *, #18001, .F. ) ;
#9130 = CARTESIAN_POINT ( 'NONE',  ( 23.32352258632852227, -0.4171737454618665297, -10.59529878620608301 ) ) ;
#9131 = AXIS2_PLACEMENT_3D ( 'NONE', #1531, #6726, #23430 ) ;
#9132 = CARTESIAN_POINT ( 'NONE',  ( 2.899999929817000055, 18.99999992981999952, 2.312669445490000216E-07 ) ) ;
#9133 = CARTESIAN_POINT ( 'NONE',  ( 15.97461056860084661, -8.975192083211494420, -5.171608217064927793 ) ) ;
#9134 = CARTESIAN_POINT ( 'NONE',  ( -19.58317126038999945, -9.245977532061999682, 5.315468033165000605 ) ) ;
#9135 = CARTESIAN_POINT ( 'NONE',  ( -14.44097954155594721, -12.31212079859721342, 3.674767524707362121 ) ) ;
#9136 = B_SPLINE_CURVE_WITH_KNOTS ( 'NONE', 3,
 ( #18847, #15319, #22710, #8192, #2620, #20910, #15561, #5774, #2136, #9525 ),
 .UNSPECIFIED., .F., .F.,
 ( 4, 2, 2, 2, 4 ),
 ( 0.000000000000000000, 0.2500000000000002220, 0.3750000000000003331, 0.5000000000000004441, 1.000000000000000000 ),
 .UNSPECIFIED. ) ;
#9137 = CARTESIAN_POINT ( 'NONE',  ( -16.77363468649999945, -9.766024879818999693, 0.2197783339474000119 ) ) ;
#9138 = CARTESIAN_POINT ( 'NONE',  ( 1.324993377608203460, 29.91963323941933695, -1.705809634641242134 ) ) ;
#9139 = ORIENTED_EDGE ( 'NONE', *, *, #583, .T. ) ;
#9140 = CARTESIAN_POINT ( 'NONE',  ( 1.812154074756000099, 25.10789601364000134, -1.214490967170999802 ) ) ;
#9141 = CARTESIAN_POINT ( 'NONE',  ( 21.66117154754112306, -2.170144149905655073, -10.48492122635746959 ) ) ;
#9142 = CARTESIAN_POINT ( 'NONE',  ( -0.8552766487867897727, 23.64350003464605265, -1.965477479697049112 ) ) ;
#9143 = ORIENTED_EDGE ( 'NONE', *, *, #21266, .T. ) ;
#9144 = CARTESIAN_POINT ( 'NONE',  ( 0.000000000000000000, 29.85000000000000142, 0.000000000000000000 ) ) ;
#9145 = CARTESIAN_POINT ( 'NONE',  ( 0.6124999999999999334, 1.217145837503000065E-14, 0.000000000000000000 ) ) ;
#9146 = EDGE_CURVE ( 'NONE', #22807, #21993, #11798, .T. ) ;
#9147 = AXIS2_PLACEMENT_3D ( 'NONE', #4344, #7857, #11735 ) ;
#9148 = MECHANICAL_DESIGN_GEOMETRIC_PRESENTATION_REPRESENTATION (  '', ( #5735 ), #17598 ) ;
#9149 = CARTESIAN_POINT ( 'NONE',  ( -4.396898345509000272, 12.25739909476000733, -2.028097624563999446 ) ) ;
#9150 = ORIENTED_EDGE ( 'NONE', *, *, #8672, .F. ) ;
#9151 = CARTESIAN_POINT ( 'NONE',  ( 13.80543875730999837, 6.427790461817999734, -6.492639392963999612 ) ) ;
#9152 = EDGE_LOOP ( 'NONE', ( #433, #138, #12263 ) ) ;
#9153 = LINE ( 'NONE', #7327, #13692 ) ;
#9154 = CARTESIAN_POINT ( 'NONE',  ( -14.45960645816625068, 2.455948253056539965, -12.49996645506552539 ) ) ;
#9155 = VERTEX_POINT ( 'NONE', #9814 ) ;
#9156 = VECTOR ( 'NONE', #18586, 1000.000000000000227 ) ;
#9157 = CARTESIAN_POINT ( 'NONE',  ( -15.61042920454667104, 4.568651703649176277, 7.926930427632896681 ) ) ;
#9158 = CARTESIAN_POINT ( 'NONE',  ( -20.15286497918999942, 1.035681084484999959, 10.55014544111999975 ) ) ;
#9159 = CARTESIAN_POINT ( 'NONE',  ( -20.23016201347000020, -9.838557159217998560, 0.7066799550067000002 ) ) ;
#9160 = CARTESIAN_POINT ( 'NONE',  ( 13.21250000000000036, 0.000000000000000000, 0.000000000000000000 ) ) ;
#9161 = DIRECTION ( 'NONE',  ( -0.9865822012466877178, 0.000000000000000000, -0.1632653061223979518 ) ) ;
#9162 = CARTESIAN_POINT ( 'NONE',  ( 0.2359769429284387376, 26.79041702683161930, -2.194852148367845146 ) ) ;
#9163 = AXIS2_PLACEMENT_3D ( 'NONE', #1821, #13189, #7621 ) ;
#9164 = CARTESIAN_POINT ( 'NONE',  ( -7.135183041691996131, 15.40308931772999479, 1.043144557813000084 ) ) ;
#9165 = CARTESIAN_POINT ( 'NONE',  ( 2.022581721832676926, 30.64951854208338133, -0.7578523236017076226 ) ) ;
#9166 = ORIENTED_EDGE ( 'NONE', *, *, #7884, .T. ) ;
#9167 = CARTESIAN_POINT ( 'NONE',  ( -18.26174577250666786, -8.901978021259040474, -2.392470463651766188 ) ) ;
#9168 = CARTESIAN_POINT ( 'NONE',  ( 3.100000000000000089, 17.00000000000000000, 0.000000000000000000 ) ) ;
#9169 = CARTESIAN_POINT ( 'NONE',  ( 13.62456398135812030, -0.2661322460768725251, -9.069200149764863994 ) ) ;
#9170 = CARTESIAN_POINT ( 'NONE',  ( 5.856952141942437962, 14.44447281020456408, -1.792848595071122597 ) ) ;
#9171 = CARTESIAN_POINT ( 'NONE',  ( 0.9439018917106000162, 28.64864211381999937, 1.852511768836999861 ) ) ;
#9172 = DIRECTION ( 'NONE',  ( 1.000000000000000000, 0.000000000000000000, 0.000000000000000000 ) ) ;
#9173 = CARTESIAN_POINT ( 'NONE',  ( 3.602888212551376146, 12.02596803873696985, 3.222497887462735022 ) ) ;
#9174 = EDGE_LOOP ( 'NONE', ( #10129, #21604, #10627, #19099, #21358 ) ) ;
#9175 = CARTESIAN_POINT ( 'NONE',  ( -2.478649635289443598, 11.74284498083996375, -4.136397467743439194 ) ) ;
#9176 = CARTESIAN_POINT ( 'NONE',  ( -10.38810889560006778, 15.62418126105870542, 1.271664699463827430 ) ) ;
#9177 = AXIS2_PLACEMENT_3D ( 'NONE', #6221, #23171, #13975 ) ;
#9178 = FACE_OUTER_BOUND ( 'NONE', #7202, .T. ) ;
#9179 = EDGE_LOOP ( 'NONE', ( #11537, #19346, #21203, #3359 ) ) ;
#9180 = EDGE_CURVE ( 'NONE', #8104, #9388, #17370, .T. ) ;
#9181 = CARTESIAN_POINT ( 'NONE',  ( 23.99062354302999722, -6.216878364870000340, 12.50000000000000000 ) ) ;
#9182 = CARTESIAN_POINT ( 'NONE',  ( -16.81976253787999909, -9.102909969768001375, 0.000000000000000000 ) ) ;
#9183 = CARTESIAN_POINT ( 'NONE',  ( 14.07768908531000207, 0.2086024747513000044, -10.15948369482999958 ) ) ;
#9184 = CARTESIAN_POINT ( 'NONE',  ( 18.82077563971644452, 6.007613805412093555, 8.527724857812813752 ) ) ;
#9185 = CARTESIAN_POINT ( 'NONE',  ( -24.37124162822026818, 2.557079873875871989, 12.50000271512793049 ) ) ;
#9186 = CYLINDRICAL_SURFACE ( 'NONE', #1133, 15.45000000000000107 ) ;
#9187 = PLANE ( 'NONE',  #412 ) ;
#9188 = CARTESIAN_POINT ( 'NONE',  ( 13.50000000000000000, -9.661799839223764508, 1.236133458592524104 ) ) ;
#9189 = VECTOR ( 'NONE', #2377, 1000.000000000000000 ) ;
#9190 = VERTEX_POINT ( 'NONE', #4007 ) ;
#9191 = CARTESIAN_POINT ( 'NONE',  ( -7.500000000000000000, 26.50000000000000000, -6.000000000000000000 ) ) ;
#9192 = CARTESIAN_POINT ( 'NONE',  ( 23.75983873544999980, 0.4422497764812000076, -10.81708341766999837 ) ) ;
#9193 = EDGE_CURVE ( 'NONE', #16256, #18376, #1378, .T. ) ;
#9194 = DIRECTION ( 'NONE',  ( 0.000000000000000000, 0.000000000000000000, -1.000000000000000000 ) ) ;
#9195 = CARTESIAN_POINT ( 'NONE',  ( -11.04281598264000053, 15.43291325263555436, 0.1613546199214205557 ) ) ;
#9196 = CARTESIAN_POINT ( 'NONE',  ( 24.50000000000000000, 0.3475903562124330604, 10.45960510830245482 ) ) ;
#9197 = CARTESIAN_POINT ( 'NONE',  ( -4.764492196990996575, 12.47350750427999166, 0.4132957174682002632 ) ) ;
#9198 = CARTESIAN_POINT ( 'NONE',  ( 1.006368030278437464, 29.14341433222939415, -1.945138833163934100 ) ) ;
#9199 = CARTESIAN_POINT ( 'NONE',  ( -3.099999776787000005, 21.99999977679100027, -5.570936493763999179E-07 ) ) ;
#9200 = EDGE_LOOP ( 'NONE', ( #12409, #12282, #20452, #13749 ) ) ;
#9201 = DIRECTION ( 'NONE',  ( 1.000000000000000000, 0.000000000000000000, 0.000000000000000000 ) ) ;
#9202 = ORIENTED_EDGE ( 'NONE', *, *, #23599, .F. ) ;
#9203 = CARTESIAN_POINT ( 'NONE',  ( -1.763881168339999750, 23.94123933040999930, 1.557685456931000134 ) ) ;
#9204 = CARTESIAN_POINT ( 'NONE',  ( -2.184465970885641539, 28.06666666666667354, 1.259047450927253120 ) ) ;
#9205 = CARTESIAN_POINT ( 'NONE',  ( 11.78693030655810503, 4.312506568627681780, -12.49999836761436356 ) ) ;
#9206 = AXIS2_PLACEMENT_3D ( 'NONE', #13782, #6641, #8227 ) ;
#9207 = DIRECTION ( 'NONE',  ( -0.7071067811864980568, -0.7071067811865969777, 1.093190268588995838E-08 ) ) ;
#9208 = CYLINDRICAL_SURFACE ( 'NONE', #16513, 2.000000000000000000 ) ;
#9209 = CARTESIAN_POINT ( 'NONE',  ( 13.09050158531000108, 2.578416522421000057, 9.802228185182000786 ) ) ;
#9210 = EDGE_CURVE ( 'NONE', #12844, #16360, #20368, .T. ) ;
#9211 = EDGE_LOOP ( 'NONE', ( #23958, #14657, #3648, #6852, #5150, #6311 ) ) ;
#9212 = CARTESIAN_POINT ( 'NONE',  ( -14.13294016288999977, 9.260019365940999947, -2.871107829034000414 ) ) ;
#9213 = DIRECTION ( 'NONE',  ( 0.000000000000000000, 1.000000000000000000, 0.000000000000000000 ) ) ;
#9214 = CONICAL_SURFACE ( 'NONE', #12320, 14.15464499511999996, 0.6126053401530057174 ) ;
#9215 = FACE_OUTER_BOUND ( 'NONE', #10385, .T. ) ;
#9216 = EDGE_LOOP ( 'NONE', ( #16773, #18764, #97, #19049 ) ) ;
#9217 = CARTESIAN_POINT ( 'NONE',  ( -10.43420619172003860, 15.58275592125444931, -1.312790953672736682 ) ) ;
#9218 = CARTESIAN_POINT ( 'NONE',  ( 2.141482600577999662, 24.89737365715999928, -0.1157515109216999960 ) ) ;
#9219 = CARTESIAN_POINT ( 'NONE',  ( 14.41906648891345455, -1.524465402106258471, -10.20485689444239519 ) ) ;
#9220 = CARTESIAN_POINT ( 'NONE',  ( 24.50000000000000000, 0.000000000000000000, 0.000000000000000000 ) ) ;
#9221 = CARTESIAN_POINT ( 'NONE',  ( 24.60268290209999975, -6.843945738500000431, 9.013297814461999735 ) ) ;
#9222 = CARTESIAN_POINT ( 'NONE',  ( 1.605714764276999995, 29.68981568338000088, -1.730281315055000046 ) ) ;
#9223 = ADVANCED_FACE ( 'NONE', ( #11521 ), #2682, .T. ) ;
#9224 = CARTESIAN_POINT ( 'NONE',  ( 13.68370378423180078, 8.311088653021329264, -3.515498294082253228 ) ) ;
#9225 = CARTESIAN_POINT ( 'NONE',  ( -6.493754939510261615, 15.47278019132436633, -1.455574667720375803 ) ) ;
#9226 = VECTOR ( 'NONE', #8002, 1000.000000000000000 ) ;
#9227 = FACE_OUTER_BOUND ( 'NONE', #21737, .T. ) ;
#9228 = VERTEX_POINT ( 'NONE', #4616 ) ;
#9229 = CARTESIAN_POINT ( 'NONE',  ( -2.531009774008887270, 24.22915547920286627, -0.09632474734362661550 ) ) ;
#9230 = CARTESIAN_POINT ( 'NONE',  ( 24.50000000000000711, -10.20164407018255837, 0.8509029801991366826 ) ) ;
#9231 = EDGE_CURVE ( 'NONE', #1224, #8048, #20473, .T. ) ;
#9232 = ORIENTED_EDGE ( 'NONE', *, *, #16595, .F. ) ;
#9233 = CARTESIAN_POINT ( 'NONE',  ( -5.372805085453999929, 16.07374366015000078, -2.940844016990000309 ) ) ;
#9234 = CARTESIAN_POINT ( 'NONE',  ( 4.750000000000000000, 15.09999999999999964, 0.000000000000000000 ) ) ;
#9235 = CARTESIAN_POINT ( 'NONE',  ( 21.34228936713000024, 9.218966921638999779, 0.000000000000000000 ) ) ;
#9236 = AXIS2_PLACEMENT_3D ( 'NONE', #10034, #17419, #2154 ) ;
#9237 = VECTOR ( 'NONE', #5089, 1000.000000000000000 ) ;
#9238 = CARTESIAN_POINT ( 'NONE',  ( 18.56154373921000200, 10.40205886901000021, -3.950313236753000279 ) ) ;
#9239 = CARTESIAN_POINT ( 'NONE',  ( -6.142995259236280425, 15.92730771963155689, 1.075595792251097693 ) ) ;
#9240 = EDGE_CURVE ( 'NONE', #20732, #15990, #15023, .T. ) ;
#9241 = CARTESIAN_POINT ( 'NONE',  ( -1.876963106047000007, 26.69506359724000077, -1.603077936557000038 ) ) ;
#9242 = ADVANCED_FACE ( 'NONE', ( #14054 ), #7306, .T. ) ;
#9243 = ORIENTED_EDGE ( 'NONE', *, *, #9240, .F. ) ;
#9244 = CARTESIAN_POINT ( 'NONE',  ( -10.91999006584999954, -12.27213681847000082, -8.393598339211999715 ) ) ;
#9245 = AXIS2_PLACEMENT_3D ( 'NONE', #16377, #7171, #16615 ) ;
#9246 = LINE ( 'NONE', #5950, #1270 ) ;
#9247 = DIRECTION ( 'NONE',  ( -1.000000000000000000, 0.000000000000000000, 0.000000000000000000 ) ) ;
#9248 = CARTESIAN_POINT ( 'NONE',  ( -12.42283980531000154, 12.23011958036999935, -9.372058967585999767 ) ) ;
#9249 = CARTESIAN_POINT ( 'NONE',  ( 23.41677564524290744, 34.01856778792605240, -6.000000000000000000 ) ) ;
#9250 = CARTESIAN_POINT ( 'NONE',  ( 23.41677564524290744, 35.51856778792605240, -6.000000000000000000 ) ) ;
#9251 = CARTESIAN_POINT ( 'NONE',  ( 16.11211489208788450, -5.644912813679614949, -8.690873081026319724 ) ) ;
#9252 = CARTESIAN_POINT ( 'NONE',  ( -15.01422961087000019, 1.689195866378999877, -10.88871722812999998 ) ) ;
#9253 = AXIS2_PLACEMENT_3D ( 'NONE', #17747, #13980, #13855 ) ;
#9254 = CARTESIAN_POINT ( 'NONE',  ( 2.000000000000000000, 18.72912878474779319, 0.000000000000000000 ) ) ;
#9255 = ADVANCED_FACE ( 'NONE', ( #21325 ), #10065, .T. ) ;
#9256 = CIRCLE ( 'NONE', #9628, 4.724999999999999645 ) ;
#9257 = CARTESIAN_POINT ( 'NONE',  ( -13.52354911898000012, -2.293961044660999704, 9.402123702338000655 ) ) ;
#9258 = CARTESIAN_POINT ( 'NONE',  ( 2.157175093438090219, 29.79162255941403359, 0.2087797654426111760 ) ) ;
#9259 = ORIENTED_EDGE ( 'NONE', *, *, #18938, .F. ) ;
#9260 = CARTESIAN_POINT ( 'NONE',  ( -2.008968276635000105, 23.78173846916000045, -0.8503130695115000970 ) ) ;
#9261 = CARTESIAN_POINT ( 'NONE',  ( 22.00165215149456444, 8.873424619505614785, -6.013099889673867438 ) ) ;
#9262 = CARTESIAN_POINT ( 'NONE',  ( -0.8767952504666675084, 23.65152616175392453, -1.964765437033486162 ) ) ;
#9263 = CIRCLE ( 'NONE', #7699, 6.125000000000002665 ) ;
#9264 = ORIENTED_EDGE ( 'NONE', *, *, #18014, .F. ) ;
#9265 = CARTESIAN_POINT ( 'NONE',  ( 0.000000000000000000, 9.100092063578999912, 0.000000000000000000 ) ) ;
#9266 = DIRECTION ( 'NONE',  ( -0.2123567536025093572, 0.9771922068863437838, 0.000000000000000000 ) ) ;
#9267 = CARTESIAN_POINT ( 'NONE',  ( 4.492400324385998012, 12.36848690438001164, -1.675184738194000378 ) ) ;
#9268 = AXIS2_PLACEMENT_3D ( 'NONE', #20725, #5714, #20499 ) ;
#9269 = EDGE_CURVE ( 'NONE', #23400, #5348, #1128, .T. ) ;
#9270 = CARTESIAN_POINT ( 'NONE',  ( 15.23137625731000000, -4.902144360783999844, -7.754105707547999771 ) ) ;
#9271 = EDGE_CURVE ( 'NONE', #14835, #21669, #4603, .T. ) ;
#9272 = VERTEX_POINT ( 'NONE', #23000 ) ;
#9273 = CIRCLE ( 'NONE', #11197, 4.649999999999999467 ) ;
#9274 = CARTESIAN_POINT ( 'NONE',  ( -14.25243324638999809, 6.216878364870000340, -12.50000000000000000 ) ) ;
#9275 = VECTOR ( 'NONE', #16329, 1000.000000000000000 ) ;
#9276 = CARTESIAN_POINT ( 'NONE',  ( -14.47125380616164492, -2.070155988435417704, -12.49997628897334501 ) ) ;
#9277 = ORIENTED_EDGE ( 'NONE', *, *, #14537, .F. ) ;
#9278 = PLANE ( 'NONE',  #8596 ) ;
#9279 = CARTESIAN_POINT ( 'NONE',  ( 12.00000000000000178, 3.168049150117523638, -8.572990016710750893 ) ) ;
#9280 = DIRECTION ( 'NONE',  ( 0.000000000000000000, 1.000000000000000000, 0.000000000000000000 ) ) ;
#9282 = EDGE_CURVE ( 'NONE', #13697, #14211, #21588, .T. ) ;
#9281 = LINE ( 'NONE', #6987, #1905 ) ;
#9283 = ADVANCED_FACE ( 'NONE', ( #22883 ), #4365, .T. ) ;
#9284 = CARTESIAN_POINT ( 'NONE',  ( -23.93282274426380596, 10.35928047437771404, 2.226158404521125345 ) ) ;
#9285 = CARTESIAN_POINT ( 'NONE',  ( -2.321186682587941696, 26.50000000000000711, -3.278664397485417492 ) ) ;
#9286 = CARTESIAN_POINT ( 'NONE',  ( -24.12232999016000079, 1.520060141252000183E-14, 0.000000000000000000 ) ) ;
#9287 = DIRECTION ( 'NONE',  ( 0.000000000000000000, 1.000000000000000000, 0.000000000000000000 ) ) ;
#9288 = CARTESIAN_POINT ( 'NONE',  ( 2.128973442807626792, 30.62540607072664400, -0.3665344719387015338 ) ) ;
#9289 = ORIENTED_EDGE ( 'NONE', *, *, #7630, .F. ) ;
#9290 = CARTESIAN_POINT ( 'NONE',  ( 1.014628930286358699, 26.27923812234717005, 1.944022540165884383 ) ) ;
#9291 = CARTESIAN_POINT ( 'NONE',  ( 1.666184814955848026, 24.76080278563852133, 1.341642937687889114 ) ) ;
#9292 = CARTESIAN_POINT ( 'NONE',  ( -22.62572616711135254, -6.492281254104476318, -8.331290678700625563 ) ) ;
#9293 = CARTESIAN_POINT ( 'NONE',  ( -0.2242450566330000117, 26.84521896305999888, -2.276798263289999902 ) ) ;
#9294 = DIRECTION ( 'NONE',  ( 0.000000000000000000, -1.000000000000000000, 0.000000000000000000 ) ) ;
#9295 = CIRCLE ( 'NONE', #22813, 12.50000000000000178 ) ;
#9296 = CARTESIAN_POINT ( 'NONE',  ( 2.236616701338915991, 11.69514058084769381, 4.269215119675235037 ) ) ;
#9297 = ORIENTED_EDGE ( 'NONE', *, *, #362, .F. ) ;
#9298 = CARTESIAN_POINT ( 'NONE',  ( -0.9309833650500990432, 11.51982210469550338, -4.721885681554473635 ) ) ;
#9299 = CARTESIAN_POINT ( 'NONE',  ( -11.04281598264000053, 15.31903517167999951, 1.878299281558999834 ) ) ;
#9300 = CARTESIAN_POINT ( 'NONE',  ( -1.904955016777212684, 29.30416709048808244, 1.249154685861223912 ) ) ;
#9301 = ORIENTED_EDGE ( 'NONE', *, *, #9146, .F. ) ;
#9302 = CARTESIAN_POINT ( 'NONE',  ( -23.75393112313999922, 13.93375672974000068, -0.5770173629729000719 ) ) ;
#9303 = CARTESIAN_POINT ( 'NONE',  ( 16.71018908530999880, 2.886377165994000293, 9.815223273854998709 ) ) ;
#9304 = CARTESIAN_POINT ( 'NONE',  ( 18.13997558517295872, 1.806292539708457934, -10.29261115798856352 ) ) ;
#9305 = CARTESIAN_POINT ( 'NONE',  ( -2.184465970885641983, 29.10086340285666751, 1.259047450927253564 ) ) ;
#9306 = CARTESIAN_POINT ( 'NONE',  ( -4.900699999999999612, 1.284663064832999817E-14, 0.000000000000000000 ) ) ;
#9307 = LINE ( 'NONE', #16442, #3536 ) ;
#9308 = CARTESIAN_POINT ( 'NONE',  ( 6.243179582884000212, 1.410249977594731933E-14, 13.77250448649344250 ) ) ;
#9309 = EDGE_LOOP ( 'NONE', ( #6070, #23511, #7659 ) ) ;
#9310 = CARTESIAN_POINT ( 'NONE',  ( -2.000000000000000000, 18.10000000000000142, 0.000000000000000000 ) ) ;
#9311 = CARTESIAN_POINT ( 'NONE',  ( 22.60328865247000252, -1.313042956010000095, 11.24729106410999968 ) ) ;
#9312 = CARTESIAN_POINT ( 'NONE',  ( 0.000000000000000000, 15.04999987253368943, -2.704938617610999654E-14 ) ) ;
#9313 = ORIENTED_EDGE ( 'NONE', *, *, #8615, .F. ) ;
#9314 = CARTESIAN_POINT ( 'NONE',  ( 13.89035753402663254, -9.969457238322348758, -2.796840301697916864 ) ) ;
#9315 = CARTESIAN_POINT ( 'NONE',  ( 24.50000000000000355, 3.444092371770813621, 9.698360394283593422 ) ) ;
#9316 = CARTESIAN_POINT ( 'NONE',  ( -4.565401903344999290, 12.39645977841000324, 1.432179347221001153 ) ) ;
#9317 = CARTESIAN_POINT ( 'NONE',  ( 1.737941468486482455, 29.08498798696146181, -1.285333566862393972 ) ) ;
#9318 = EDGE_CURVE ( 'NONE', #10616, #11620, #966, .T. ) ;
#9319 = CARTESIAN_POINT ( 'NONE',  ( -21.64241867476000181, 8.060209368933000107, 7.624942817855999699 ) ) ;
#9320 = ORIENTED_EDGE ( 'NONE', *, *, #5722, .F. ) ;
#9321 = CARTESIAN_POINT ( 'NONE',  ( 1.699994387327691481, 10.36668292280599957, 1.053574431676630008 ) ) ;
#9322 = ORIENTED_EDGE ( 'NONE', *, *, #13368, .T. ) ;
#9323 = CARTESIAN_POINT ( 'NONE',  ( 1.678513321804000036, 24.15025016897999777, 1.649317033692999868 ) ) ;
#9324 = CARTESIAN_POINT ( 'NONE',  ( 5.358355417570997759, 14.28398881512000607, 2.883859362742000165 ) ) ;
#9325 = CARTESIAN_POINT ( 'NONE',  ( 16.05145603379665431, 7.936819607890199357, 4.574351470713802215 ) ) ;
#9326 = CARTESIAN_POINT ( 'NONE',  ( 0.000000000000000000, 18.89999999999999858, 0.000000000000000000 ) ) ;
#9327 = FACE_OUTER_BOUND ( 'NONE', #16218, .T. ) ;
#9328 = CARTESIAN_POINT ( 'NONE',  ( 14.73581408531000037, 7.589869243736000470, 6.782654363299000622 ) ) ;
#9329 =( NAMED_UNIT ( * ) PLANE_ANGLE_UNIT ( ) SI_UNIT ( $, .RADIAN. ) );
#9330 = CARTESIAN_POINT ( 'NONE',  ( -12.37247714714999880, 8.083715232074000667, -4.229267010826999851 ) ) ;
#9331 = B_SPLINE_CURVE_WITH_KNOTS ( 'NONE', 3,
 ( #4543, #12300, #7077, #23549, #19687, #23418, #21971, #6960, #1629, #18113, #3104, #6713, #9019, #14104, #16149, #12425, #12771, #14229 ),
 .UNSPECIFIED., .F., .F.,
 ( 4, 2, 2, 2, 2, 2, 2, 2, 4 ),
 ( 0.000000000000000000, 0.1249999999999999722, 0.2500000000000000000, 0.3750000000000000000, 0.5000000000000000000, 0.6250000000000000000, 0.7499999999999998890, 0.8750000000000000000, 1.000000000000000000 ),
 .UNSPECIFIED. ) ;
#9332 = FACE_OUTER_BOUND ( 'NONE', #4010, .T. ) ;
#9333 = LINE ( 'NONE', #17186, #13223 ) ;
#9334 = ORIENTED_EDGE ( 'NONE', *, *, #20798, .F. ) ;
#9335 = CARTESIAN_POINT ( 'NONE',  ( -10.04701370327999932, 16.31160201366999729, -1.000000000000000000 ) ) ;
#9336 = CARTESIAN_POINT ( 'NONE',  ( 1.820465805901000156, 24.96141477156000121, -1.133688841959000104 ) ) ;
#9337 = CARTESIAN_POINT ( 'NONE',  ( 14.57889531702554464, 4.053392352543252031, -9.495965673588385059 ) ) ;
#9338 = CARTESIAN_POINT ( 'NONE',  ( -17.91572087121334178, 7.301875228516277794, -5.611357487623554796 ) ) ;
#9339 = CARTESIAN_POINT ( 'NONE',  ( 20.19755579089999742, 9.974711832087001184, -5.086754361666000257 ) ) ;
#9340 = CARTESIAN_POINT ( 'NONE',  ( 2.226929716040000340, 28.82810905619000152, -0.7829338363701999759 ) ) ;
#9341 = CARTESIAN_POINT ( 'NONE',  ( 13.82849600701260862, 9.024859065751403620, 0.8634124378813970990 ) ) ;
#9342 = CARTESIAN_POINT ( 'NONE',  ( 3.163367236287002005, 12.09434266441998673, -3.669474972920002909 ) ) ;
#9343 = EDGE_CURVE ( 'NONE', #8899, #6464, #2802, .T. ) ;
#9344 = CARTESIAN_POINT ( 'NONE',  ( 19.55914433211999892, -7.278973637726999790, -8.742471291912998765 ) ) ;
#9345 = ORIENTED_EDGE ( 'NONE', *, *, #12310, .F. ) ;
#9346 = CARTESIAN_POINT ( 'NONE',  ( 2.000000000000000000, 30.00000000000000000, -3.464101615137999968 ) ) ;
#9347 = EDGE_LOOP ( 'NONE', ( #23672, #11409, #6434, #14239, #3119 ) ) ;
#9348 = CARTESIAN_POINT ( 'NONE',  ( -16.14541243917331315, -2.378020554675936982, -8.849179423685832546 ) ) ;
#9349 = CARTESIAN_POINT ( 'NONE',  ( 24.34804274388850587, 9.160073233599486997, 9.134287758352421349 ) ) ;
#9350 = DIRECTION ( 'NONE',  ( 0.000000000000000000, 1.000000000000000000, 0.000000000000000000 ) ) ;
#9351 = CARTESIAN_POINT ( 'NONE',  ( 18.59537304017000281, 10.74774789134999864, 2.883182032014000029 ) ) ;
#9352 = PLANE ( 'NONE',  #19514 ) ;
#9353 = CARTESIAN_POINT ( 'NONE',  ( 1.994688225595000253, 25.52506359724000262, 1.016344414748000080 ) ) ;
#9354 = EDGE_CURVE ( 'NONE', #11075, #20732, #8365, .T. ) ;
#9355 = VERTEX_POINT ( 'NONE', #4741 ) ;
#9356 = ORIENTED_EDGE ( 'NONE', *, *, #14726, .F. ) ;
#9357 = CARTESIAN_POINT ( 'NONE',  ( -11.73457006584999895, 14.06883258501999912, 4.808938159164000581 ) ) ;
#9358 = CARTESIAN_POINT ( 'NONE',  ( 1.139388574200934423, 6.872381371660192251, -1.333228779845821776 ) ) ;
#9359 = DIRECTION ( 'NONE',  ( -0.000000000000000000, 1.000000000000000000, -0.000000000000000000 ) ) ;
#9360 = ORIENTED_EDGE ( 'NONE', *, *, #20628, .T. ) ;
#9361 = CARTESIAN_POINT ( 'NONE',  ( -24.43506354683046311, 9.928196662808350226, 7.803922592516721046 ) ) ;
#9362 = CARTESIAN_POINT ( 'NONE',  ( 0.000000000000000000, 17.00000000000000000, 0.000000000000000000 ) ) ;
#9363 = CARTESIAN_POINT ( 'NONE',  ( 6.240092085251032650, 13.67838160267347014, 1.680192384702403618 ) ) ;
#9364 = CARTESIAN_POINT ( 'NONE',  ( 15.93200848183689722, -9.659035961499510492, -3.741044914201433702 ) ) ;
#9365 = CARTESIAN_POINT ( 'NONE',  ( -18.37874916017999638, 9.689337229684999997, 5.438183135797000745 ) ) ;
#9366 = CARTESIAN_POINT ( 'NONE',  ( 2.146824282253999794, 30.41473571554000088, -0.4462322471723000339 ) ) ;
#9367 = VECTOR ( 'NONE', #10685, 1000.000000000000000 ) ;
#9368 = B_SPLINE_CURVE_WITH_KNOTS ( 'NONE', 3,
 ( #9611, #2343, #4286, #7796, #9732, #13129, #11437, #18813, #2458, #19048, #13594, #15168, #15282, #3929, #13241, #20991, #159, #22796, #5968, #18696, #20878, #13351, #8033, #4402, #15053, #11793, #1990, #9375, #16747, #20751, #14928, #4162, #11322, #18936, #2105, #9494, #21480, #17857, #10214, #2954, #19670, #21357, #12158, #2711, #4894, #10342, #8280, #8403, #17481, #17607, #17356, #23399, #12281, #23280, #13715, #876, #9969, #17732, #1132, #6332, #3083, #1251, #23035, #15643, #10469, #21111, #21239, #4652, #15771, #4524, #8160, #11915, #759, #14085, #1002, #15527, #8531, #10094, #19170, #6453, #19298, #23160, #15889, #13840, #12039, #19422, #8641, #16005, #6817, #2834, #6693, #6579, #13963, #14209, #22914, #21606, #4773, #19548, #5023, #2579, #10702, #14676, #1498, #20258, #5478, #7403 ),
 .UNSPECIFIED., .F., .F.,
 ( 4, 2, 1, 2, 2, 2, 2, 2, 2, 2, 2, 2, 2, 2, 1, 2, 2, 2, 2, 2, 2, 2, 2, 2, 2, 2, 1, 2, 2, 2, 2, 2, 2, 2, 2, 2, 1, 2, 1, 2, 2, 2, 2, 2, 2, 2, 2, 2, 1, 2, 2, 2, 2, 2, 2, 4 ),
 ( 0.000000000000000000, 0.01562500000000000000, 0.03125000000000000000, 0.04687500000000000000, 0.06250000000000000000, 0.07812500000000000000, 0.09375000000000000000, 0.1250000000000000000, 0.1562500000000000000, 0.1718750000000000000, 0.1875000000000000000, 0.2031250000000000000, 0.2187500000000000000, 0.2343750000000000000, 0.2500000000000000000, 0.2656250000000000000, 0.2812500000000000000, 0.2968750000000000000, 0.3125000000000000000, 0.3437500000000000000, 0.3750000000000000000, 0.3906250000000000000, 0.4062500000000000000, 0.4218750000000000000, 0.4375000000000000000, 0.4531250000000000000, 0.4687500000000000000, 0.4843750000000000000, 0.5000000000000000000, 0.5156250000000000000, 0.5312500000000000000, 0.5625000000000000000, 0.5937500000000000000, 0.6093750000000000000, 0.6250000000000000000, 0.6406250000000000000, 0.6562500000000000000, 0.6718750000000000000, 0.6875000000000000000, 0.7031250000000000000, 0.7187500000000000000, 0.7343750000000000000, 0.7500000000000000000, 0.7812500000000000000, 0.8125000000000000000, 0.8281250000000000000, 0.8437500000000000000, 0.8593750000000000000, 0.8750000000000000000, 0.8906250000000000000, 0.9062500000000000000, 0.9218750000000000000, 0.9375000000000000000, 0.9531250000000000000, 0.9687500000000000000, 1.000000000000000000 ),
 .UNSPECIFIED. ) ;
#9369 = CARTESIAN_POINT ( 'NONE',  ( -14.01132597738000030, -2.550904266876999671, 10.45586863968000024 ) ) ;
#9370 = EDGE_CURVE ( 'NONE', #15451, #20779, #15419, .T. ) ;
#9371 = CARTESIAN_POINT ( 'NONE',  ( 1.464084226283197454, 29.69852001067018676, 1.588251168237700739 ) ) ;
#9372 = VERTEX_POINT ( 'NONE', #1690 ) ;
#9373 = CARTESIAN_POINT ( 'NONE',  ( -1.732027827905000095, 24.54951388964999737, -1.326261777753000137 ) ) ;
#9374 = CARTESIAN_POINT ( 'NONE',  ( 20.27087574806811432, 10.03231373101404600, -3.158548254409779599 ) ) ;
#9375 = CARTESIAN_POINT ( 'NONE',  ( -18.16722892299935310, 2.522433974171974569, 10.24789558780088328 ) ) ;
#9376 = EDGE_LOOP ( 'NONE', ( #21836, #8974, #339, #3635 ) ) ;
#9377 =( BOUNDED_CURVE ( )  B_SPLINE_CURVE ( 3, ( #21373, #4789, #3222, #19565, #2969, #10359, #17748, #6709, #23416, #14102 ),
 .UNSPECIFIED., .F., .F. ) 
 B_SPLINE_CURVE_WITH_KNOTS ( ( 4, 1, 1, 1, 1, 1, 1, 4 ),
 ( 0.000000000000000000, 0.07930571573750974657, 0.2537389680230056066, 0.4205310468338411267, 0.5688359795437202271, 0.7038386765312832916, 0.8425724330419954722, 1.000000000000000000 ),
 .UNSPECIFIED. ) 
 CURVE ( )  GEOMETRIC_REPRESENTATION_ITEM ( )  RATIONAL_B_SPLINE_CURVE ( ( 1.254793930016049108, 1.254793930016049108, 1.254793930016048886, 1.254793930016049108, 1.254793930016049108, 1.254793930016049108, 1.254793930016049108, 1.254793930016049108, 1.254793930016049108, 1.254793930016049108 ) ) 
 REPRESENTATION_ITEM ( '' )  );
#9378 = DIRECTION ( 'NONE',  ( 0.8500000000000165201, 0.000000000000000000, -0.5267826876426102700 ) ) ;
#9379 = CARTESIAN_POINT ( 'NONE',  ( -4.787147458302001723, 13.37298724219999002, 4.939277822045997191 ) ) ;
#9380 = CARTESIAN_POINT ( 'NONE',  ( -13.99999999999999467, -10.14973060463748666, 1.779624900529133580 ) ) ;
#9381 = EDGE_CURVE ( 'NONE', #8812, #12420, #6939, .T. ) ;
#9382 = CARTESIAN_POINT ( 'NONE',  ( 17.12250142130999819, -8.875724825267999663, -3.992994992864999926 ) ) ;
#9383 = ORIENTED_EDGE ( 'NONE', *, *, #23886, .T. ) ;
#9384 = AXIS2_PLACEMENT_3D ( 'NONE', #3996, #15115, #4 ) ;
#9385 = CARTESIAN_POINT ( 'NONE',  ( -4.309862785505534255, 15.29405002130709867, 4.352518930625178584 ) ) ;
#9386 = CARTESIAN_POINT ( 'NONE',  ( 1.999167105995457661, 29.91666666666667496, 1.536366799937278760 ) ) ;
#9387 = PRODUCT_DEFINITION_SHAPE ( 'NONE', 'NONE',  #23973 ) ;
#9388 = VERTEX_POINT ( 'NONE', #7136 ) ;
#9389 = CARTESIAN_POINT ( 'NONE',  ( 22.74058103379666917, 1.211330063708936589, -9.254849841694738899 ) ) ;
#9390 = CARTESIAN_POINT ( 'NONE',  ( 4.736790957010000191, 12.61336852909998996, -0.1514267026985999243 ) ) ;
#9391 = CARTESIAN_POINT ( 'NONE',  ( -21.01239991986000177, 8.969540160325998102, 3.381244718297999885 ) ) ;
#9392 = CARTESIAN_POINT ( 'NONE',  ( -14.43045988485367914, 9.209646829417284408, -9.048410431339574345 ) ) ;
#9393 = FACE_OUTER_BOUND ( 'NONE', #4774, .T. ) ;
#9394 = B_SPLINE_CURVE_WITH_KNOTS ( 'NONE', 3,
 ( #7731, #22728, #6142, #13531, #690, #19098, #13287, #21041 ),
 .UNSPECIFIED., .F., .F.,
 ( 4, 2, 2, 4 ),
 ( 0.000000000000000000, 0.2499999999999998890, 0.4999999999999997780, 1.000000000000000000 ),
 .UNSPECIFIED. ) ;
#9395 = CARTESIAN_POINT ( 'NONE',  ( -21.07622378627610615, -8.171794258342258033, -6.628154887273959517 ) ) ;
#9396 = FACE_OUTER_BOUND ( 'NONE', #5232, .T. ) ;
#9397 = CARTESIAN_POINT ( 'NONE',  ( -8.099999999999999645, 1.323843189878000027E-14, 0.000000000000000000 ) ) ;
#9398 = CARTESIAN_POINT ( 'NONE',  ( -10.25814758309999952, 1.350272875175999940E-14, 0.000000000000000000 ) ) ;
#9399 = EDGE_CURVE ( 'NONE', #3069, #3157, #6560, .T. ) ;
#9400 = CARTESIAN_POINT ( 'NONE',  ( 0.3983959897931292904, 30.42739071784584937, 2.122834239064325779 ) ) ;
#9401 = ORIENTED_EDGE ( 'NONE', *, *, #9712, .F. ) ;
#9402 = EDGE_CURVE ( 'NONE', #1014, #9699, #23620, .T. ) ;
#9403 = CARTESIAN_POINT ( 'NONE',  ( -17.95941243917332741, -2.390205132071402616, -8.894518645773471732 ) ) ;
#9404 = CARTESIAN_POINT ( 'NONE',  ( 12.52688711657000020, -6.216878364870000340, -12.50000000000000000 ) ) ;
#9405 = CARTESIAN_POINT ( 'NONE',  ( 1.656631363487247821, 24.76418780987420476, 1.348065658398109434 ) ) ;
#9406 = CIRCLE ( 'NONE', #22922, 2.399999999999999911 ) ;
#9407 = CARTESIAN_POINT ( 'NONE',  ( -23.42901741772625712, 3.156775733565070574, 10.10315730872225792 ) ) ;
#9408 = CARTESIAN_POINT ( 'NONE',  ( -1.556103512505999875, 26.89364211382000036, 1.683383295848999817 ) ) ;
#9409 = CARTESIAN_POINT ( 'NONE',  ( 0.000000000000000000, 18.00000000000000000, 0.000000000000000000 ) ) ;
#9410 = CARTESIAN_POINT ( 'NONE',  ( 3.136507135182145412, 11.89683589971509825, 3.669855009401824741 ) ) ;
#9411 = ORIENTED_EDGE ( 'NONE', *, *, #7770, .F. ) ;
#9412 = CARTESIAN_POINT ( 'NONE',  ( -0.7552438104605452285, 11.50694251763714604, -4.753202236774020761 ) ) ;
#9413 = EDGE_CURVE ( 'NONE', #11582, #2323, #19312, .T. ) ;
#9414 = CARTESIAN_POINT ( 'NONE',  ( 24.37705598205755209, 9.806549756205852120, -0.9735673311825817633 ) ) ;
#9415 = ADVANCED_FACE ( 'NONE', ( #12721 ), #16788, .T. ) ;
#9416 = CARTESIAN_POINT ( 'NONE',  ( 4.000000000000000000, 29.69999999999999929, -2.309401076759000304 ) ) ;
#9417 = B_SPLINE_CURVE_WITH_KNOTS ( 'NONE', 3,
 ( #15598, #23477, #13914, #6888, #22985, #8715, #16079, #19619, #8593, #6400, #21185, #2656 ),
 .UNSPECIFIED., .F., .F.,
 ( 4, 2, 2, 2, 2, 4 ),
 ( 0.000000000000000000, 0.2500000000000424660, 0.3750000000000640599, 0.4375000000000685563, 0.5000000000000730527, 1.000000000000000000 ),
 .UNSPECIFIED. ) ;
#9418 = ORIENTED_EDGE ( 'NONE', *, *, #9118, .F. ) ;
#9419 = CARTESIAN_POINT ( 'NONE',  ( -9.000000000000000000, 19.50000000000000000, -6.000000000000000000 ) ) ;
#9420 = CARTESIAN_POINT ( 'NONE',  ( 15.17456408531000100, -6.393444021559000490, 7.935320769223000781 ) ) ;
#9421 = CARTESIAN_POINT ( 'NONE',  ( 18.07176995288481081, -0.6453614156608961094, -10.39397914006448431 ) ) ;
#9422 = CARTESIAN_POINT ( 'NONE',  ( 4.000000000000117240, 27.99999999999975486, 0.1904558375517787505 ) ) ;
#9423 = CARTESIAN_POINT ( 'NONE',  ( 1.961083286043999951, 30.48982497936000158, 0.8831193726211999939 ) ) ;
#9424 = CARTESIAN_POINT ( 'NONE',  ( 17.15614037306000128, 8.095712735332998733, 7.236596325106999572 ) ) ;
#9425 = VECTOR ( 'NONE', #4171, 1000.000000000000000 ) ;
#9426 = DIRECTION ( 'NONE',  ( -1.000000000000000000, 0.000000000000000000, 0.000000000000000000 ) ) ;
#9427 = EDGE_LOOP ( 'NONE', ( #2588, #1085, #13935, #20879 ) ) ;
#9428 = DIRECTION ( 'NONE',  ( 0.000000000000000000, 0.000000000000000000, -1.000000000000000000 ) ) ;
#9429 = CARTESIAN_POINT ( 'NONE',  ( 21.36394493738999856, -9.707274230039999452, -5.764439021661999618 ) ) ;
#9430 = CARTESIAN_POINT ( 'NONE',  ( 2.434931691670793263, 29.16666666666666430, 0.6543697108981857413 ) ) ;
#9431 = ORIENTED_EDGE ( 'NONE', *, *, #13521, .T. ) ;
#9432 = CARTESIAN_POINT ( 'NONE',  ( 11.59627693011999838, -8.493620999052001963, -2.880788490115999689 ) ) ;
#9433 = DIRECTION ( 'NONE',  ( 1.000000000000000000, 0.000000000000000000, 0.000000000000000000 ) ) ;
#9434 = CARTESIAN_POINT ( 'NONE',  ( -0.1161258160197999739, 11.43408742862999716, 4.868089096411000405 ) ) ;
#9435 = CARTESIAN_POINT ( 'NONE',  ( 0.2973647920025167535, 29.18612839175506934, -2.139422557246009937 ) ) ;
#9436 = CARTESIAN_POINT ( 'NONE',  ( -22.81201049522999824, -10.99897752496999992, 1.683594084091999843 ) ) ;
#9437 = ORIENTED_EDGE ( 'NONE', *, *, #21426, .T. ) ;
#9438 = CARTESIAN_POINT ( 'NONE',  ( -2.051647590440843327, 23.66978687261612890, 0.7531949266739137450 ) ) ;
#9439 = ORIENTED_EDGE ( 'NONE', *, *, #2730, .F. ) ;
#9440 = AXIS2_PLACEMENT_3D ( 'NONE', #1024, #11815, #2855 ) ;
#9441 = CARTESIAN_POINT ( 'NONE',  ( -1.344835081562999912, 25.22921029035000018, -1.691883008907999919 ) ) ;
#9442 = CARTESIAN_POINT ( 'NONE',  ( 1.999167105995457661, 28.31666666666666998, 1.536366799937278760 ) ) ;
#9443 = DIRECTION ( 'NONE',  ( 0.5000000000000169864, 0.000000000000000000, -0.8660254037844289376 ) ) ;
#9444 = CARTESIAN_POINT ( 'NONE',  ( 0.000000000000000000, -1.550000000000000044, 0.000000000000000000 ) ) ;
#9445 = DIRECTION ( 'NONE',  ( -0.000000000000000000, 1.000000000000000000, 0.000000000000000000 ) ) ;
#9446 = LINE ( 'NONE', #111, #20770 ) ;
#9447 = CARTESIAN_POINT ( 'NONE',  ( 14.32350174931000097, 0.2192049860668999761, -10.67495121044000150 ) ) ;
#9448 = CARTESIAN_POINT ( 'NONE',  ( -14.41758667332000066, 9.911104062797001291, 4.224474430483999399 ) ) ;
#9449 = LINE ( 'NONE', #20704, #2428 ) ;
#9450 = CARTESIAN_POINT ( 'NONE',  ( 0.000000000000000000, 22.00000000000000000, 0.000000000000000000 ) ) ;
#9451 = PRODUCT_RELATED_PRODUCT_CATEGORY ( 'part', '', ( #15579 ) ) ;
#9452 = ORIENTED_EDGE ( 'NONE', *, *, #1870, .T. ) ;
#9453 = CARTESIAN_POINT ( 'NONE',  ( -10.08825016236975181, 16.08144774604313199, -1.020021333861736101 ) ) ;
#9454 = CARTESIAN_POINT ( 'NONE',  ( -1.271387008224000192, 25.40970257236000052, 1.727113330389000057 ) ) ;
#9455 = CARTESIAN_POINT ( 'NONE',  ( 13.97482487491021175, -10.24735112816637184, 1.245669702648658506 ) ) ;
#9456 = AXIS2_PLACEMENT_3D ( 'NONE', #9725, #17107, #6075 ) ;
#9457 = CARTESIAN_POINT ( 'NONE',  ( 0.000000000000000000, 29.85000000000000142, 4.309401076758999416 ) ) ;
#9458 = CARTESIAN_POINT ( 'NONE',  ( 21.81255309151999811, -1.099163774157999818, -11.18733577289999914 ) ) ;
#9459 = CARTESIAN_POINT ( 'NONE',  ( -2.015416341576000026, 29.11534459859000279, -1.228938668624000030 ) ) ;
#9460 = CARTESIAN_POINT ( 'NONE',  ( 13.60815662951419469, 7.077589705154139210, -5.594308489612157764 ) ) ;
#9461 = DIRECTION ( 'NONE',  ( 0.000000000000000000, 1.000000000000000000, 0.000000000000000000 ) ) ;
#9462 = CARTESIAN_POINT ( 'NONE',  ( -6.678873158505115981, 15.36510622990475738, 1.676819129351728055 ) ) ;
#9463 = CARTESIAN_POINT ( 'NONE',  ( 23.03766113620000056, -10.74194406456000017, -4.027689622328000318 ) ) ;
#9464 = EDGE_LOOP ( 'NONE', ( #11125, #14662 ) ) ;
#9465 = CARTESIAN_POINT ( 'NONE',  ( 0.8794326344061793588, 24.47914381499106184, 2.375062700745428135 ) ) ;
#9466 = CARTESIAN_POINT ( 'NONE',  ( 12.40357033522256280, -13.79529643152775087, 1.105845675118881211 ) ) ;
#9467 = ORIENTED_EDGE ( 'NONE', *, *, #5556, .T. ) ;
#9468 = CARTESIAN_POINT ( 'NONE',  ( -16.44774577250665004, -8.856638799171403065, -2.380285886256298777 ) ) ;
#9469 = CARTESIAN_POINT ( 'NONE',  ( 0.000000000000000000, 28.00000000000000000, 0.000000000000000000 ) ) ;
#9470 = CARTESIAN_POINT ( 'NONE',  ( 1.460999620166917756, 24.69858516586207386, 1.653668814814927890 ) ) ;
#9471 = CARTESIAN_POINT ( 'NONE',  ( 16.61041316388000055, 10.47570988103000111, -3.588975773298999972 ) ) ;
#9472 = DIRECTION ( 'NONE',  ( 0.000000000000000000, -1.000000000000000000, 0.000000000000000000 ) ) ;
#9473 = CARTESIAN_POINT ( 'NONE',  ( 0.05241653317065999435, 26.88212896666999896, 2.669209039122999894 ) ) ;
#9474 = ORIENTED_EDGE ( 'NONE', *, *, #10428, .F. ) ;
#9475 = VERTEX_POINT ( 'NONE', #4670 ) ;
#9476 = CARTESIAN_POINT ( 'NONE',  ( -10.49795221169000037, 10.03457821036000119, 11.90362028209000123 ) ) ;
#9477 = CARTESIAN_POINT ( 'NONE',  ( -4.000000000000000000, 24.50000000000000000, 0.000000000000000000 ) ) ;
#9478 = CARTESIAN_POINT ( 'NONE',  ( 17.71428936713000013, 9.125865291226999076, 0.000000000000000000 ) ) ;
#9479 = EDGE_CURVE ( 'NONE', #18038, #11323, #15044, .T. ) ;
#9480 = VERTEX_POINT ( 'NONE', #17622 ) ;
#9481 = CARTESIAN_POINT ( 'NONE',  ( -5.529771451991000397, 1.198997689148999791E-14, 1.310996564781999865E-13 ) ) ;
#9482 = CARTESIAN_POINT ( 'NONE',  ( 19.61728472050814176, -3.208866004501119473, -10.00333024590596054 ) ) ;
#9483 = PLANE ( 'NONE',  #6807 ) ;
#9484 = CARTESIAN_POINT ( 'NONE',  ( 15.59175458660710056, -7.210646299692904826, 7.423952708739454565 ) ) ;
#9485 = CARTESIAN_POINT ( 'NONE',  ( -17.87080093323000085, -2.119561155269000352, 10.89291255152999938 ) ) ;
#9486 = CARTESIAN_POINT ( 'NONE',  ( 0.5124189445521000197, 30.55860975689000014, -2.131997105840000017 ) ) ;
#9487 = VECTOR ( 'NONE', #22519, 1000.000000000000000 ) ;
#9488 = CARTESIAN_POINT ( 'NONE',  ( -19.29271502458999876, -7.174960688273000819, 7.031698840148000507 ) ) ;
#9489 = EDGE_CURVE ( 'NONE', #13414, #13163, #9730, .T. ) ;
#9490 = CARTESIAN_POINT ( 'NONE',  ( -0.2454928412648832159, 29.58943779370164151, 2.147640904564822151 ) ) ;
#9491 = ORIENTED_EDGE ( 'NONE', *, *, #11278, .T. ) ;
#9492 = CARTESIAN_POINT ( 'NONE',  ( 2.261417238927000195, 24.18218325944999947, 0.5843056356417000163 ) ) ;
#9493 = CARTESIAN_POINT ( 'NONE',  ( 0.000000000000000000, 22.09999988306816832, -4.649999883068000273 ) ) ;
#9494 = CARTESIAN_POINT ( 'NONE',  ( -17.76208048912187110, -9.713398265221545813, 4.231666101567703286 ) ) ;
#9495 = VERTEX_POINT ( 'NONE', #4539 ) ;
#9496 = CARTESIAN_POINT ( 'NONE',  ( 24.50000000000000000, 0.000000000000000000, 12.50000000000000000 ) ) ;
#9497 = DIRECTION ( 'NONE',  ( 0.000000000000000000, 0.000000000000000000, 1.000000000000000000 ) ) ;
#9498 = DIRECTION ( 'NONE',  ( 0.000000000000000000, -0.5000000000000169864, -0.8660254037844288266 ) ) ;
#9499 = VECTOR ( 'NONE', #4540, 1000.000000000000000 ) ;
#9500 = CARTESIAN_POINT ( 'NONE',  ( 14.90231375730999908, -9.084442286569000657, 1.213034410125000129 ) ) ;
#9501 = ORIENTED_EDGE ( 'NONE', *, *, #2676, .F. ) ;
#9502 = CONICAL_SURFACE ( 'NONE', #3339, 3.049999825846000157, 0.7853981633972997312 ) ;
#9503 = CARTESIAN_POINT ( 'NONE',  ( -4.739682122679631959, 15.68822824407284067, 3.880277545986481336 ) ) ;
#9504 = CARTESIAN_POINT ( 'NONE',  ( 24.18393254356861632, -13.26880198692879276, 2.017760803068382458 ) ) ;
#9505 = EDGE_CURVE ( 'NONE', #23934, #21619, #8477, .T. ) ;
#9506 = VERTEX_POINT ( 'NONE', #8419 ) ;
#9507 = CARTESIAN_POINT ( 'NONE',  ( -15.72380420454666528, 7.256715315803072386, 5.576969440672721490 ) ) ;
#9508 = CARTESIAN_POINT ( 'NONE',  ( 4.501062182727002536, 12.52238982561000746, 1.504078967853000881 ) ) ;
#9509 = CARTESIAN_POINT ( 'NONE',  ( 12.00000000000000178, -4.050809156854140447, -8.703506550480188508 ) ) ;
#9510 = DIRECTION ( 'NONE',  ( 0.000000000000000000, 0.000000000000000000, 1.000000000000000000 ) ) ;
#9511 = CYLINDRICAL_SURFACE ( 'NONE', #18158, 1.000000000000000222 ) ;
#9512 = DIRECTION ( 'NONE',  ( 0.000000000000000000, 0.000000000000000000, -1.000000000000000000 ) ) ;
#9513 = CARTESIAN_POINT ( 'NONE',  ( 2.500000000000000000, 28.65086340285666111, -0.3272492347489373565 ) ) ;
#9514 = LINE ( 'NONE', #4426, #2193 ) ;
#9515 = EDGE_CURVE ( 'NONE', #8048, #21798, #22767, .T. ) ;
#9516 = CARTESIAN_POINT ( 'NONE',  ( 2.146464929684074541, 30.58969480563138887, 0.2409270991070303070 ) ) ;
#9517 = VERTEX_POINT ( 'NONE', #10358 ) ;
#9518 = CARTESIAN_POINT ( 'NONE',  ( -18.07278743917332875, -5.613834502798916049, -7.305098395835319280 ) ) ;
#9519 = CARTESIAN_POINT ( 'NONE',  ( 24.09204327667999834, -8.784117800967999656, 5.624662619288000265 ) ) ;
#9520 = CARTESIAN_POINT ( 'NONE',  ( 13.53123041467663334, -3.132728285495402609, -8.512962057649877679 ) ) ;
#9521 = CARTESIAN_POINT ( 'NONE',  ( 2.434931691670791487, 27.80086340285666680, 0.6543697108981911814 ) ) ;
#9522 = CARTESIAN_POINT ( 'NONE',  ( -22.83993716727533041, -10.41765305974887035, -1.759783978785091296 ) ) ;
#9523 = CARTESIAN_POINT ( 'NONE',  ( 0.04836512055258999909, 27.02446440326000143, 2.462898805936000191 ) ) ;
#9524 = CIRCLE ( 'NONE', #21131, 10.50000000000000000 ) ;
#9525 = CARTESIAN_POINT ( 'NONE',  ( -6.637070260807000466, 26.35799170939839797, 1.000000000000000000 ) ) ;
#9526 = EDGE_LOOP ( 'NONE', ( #2427, #17766, #8928, #8798 ) ) ;
#9527 = ADVANCED_FACE ( 'NONE', ( #15787 ), #2968, .F. ) ;
#9528 = CARTESIAN_POINT ( 'NONE',  ( 0.5604879404901262907, 11.49595935512666678, -4.779696783358256873 ) ) ;
#9529 = CARTESIAN_POINT ( 'NONE',  ( -2.693005968609320178, 29.96241504948189416, 3.063994432611676366 ) ) ;
#9530 = DIRECTION ( 'NONE',  ( 0.000000000000000000, 1.000000000000000000, 0.000000000000000000 ) ) ;
#9531 = B_SPLINE_CURVE_WITH_KNOTS ( 'NONE', 3,
 ( #11772, #4499, #8506, #19273, #19525, #608, #17331, #4752, #8010, #6309, #13694, #22772, #12136, #19399, #6672, #11654, #15747, #10075 ),
 .UNSPECIFIED., .F., .F.,
 ( 4, 2, 2, 2, 2, 2, 2, 2, 4 ),
 ( 0.000000000000000000, 0.1250000000000000000, 0.2500000000000000000, 0.3750000000000000000, 0.5000000000000000000, 0.6250000000000000000, 0.7500000000000000000, 0.8750000000000000000, 1.000000000000000000 ),
 .UNSPECIFIED. ) ;
#9532 = VERTEX_POINT ( 'NONE', #6348 ) ;
#9533 = ADVANCED_FACE ( 'NONE', ( #8295 ), #19317, .T. ) ;
#9534 = EDGE_CURVE ( 'NONE', #10909, #13113, #16210, .T. ) ;
#9535 = DIRECTION ( 'NONE',  ( 0.000000000000000000, 1.000000000000000000, 0.000000000000000000 ) ) ;
#9536 = AXIS2_PLACEMENT_3D ( 'NONE', #21547, #15950, #6637 ) ;
#9537 = CARTESIAN_POINT ( 'NONE',  ( 12.87112658530999987, 8.616207371593000985, 5.326914196072999985 ) ) ;
#9538 = CARTESIAN_POINT ( 'NONE',  ( -19.01635896142999727, -2.665689585159999986, -11.12245455963000040 ) ) ;
#9539 = PLANE ( 'NONE',  #10424 ) ;
#9540 = CARTESIAN_POINT ( 'NONE',  ( 15.66608580085999947, -10.66676427418000017, 3.898330567911000077 ) ) ;
#9541 = FACE_OUTER_BOUND ( 'NONE', #21506, .T. ) ;
#9542 = CARTESIAN_POINT ( 'NONE',  ( -1.536366799937282313, 26.75086340285667319, 1.999167105995454552 ) ) ;
#9543 = CARTESIAN_POINT ( 'NONE',  ( 21.11556404106000073, 9.695547301195000856, -0.01981028907428000058 ) ) ;
#9544 = EDGE_CURVE ( 'NONE', #2323, #13406, #13878, .T. ) ;
#9545 = DIRECTION ( 'NONE',  ( 1.000000000000000000, 0.000000000000000000, -2.391341176003999979E-11 ) ) ;
#9546 = ORIENTED_EDGE ( 'NONE', *, *, #11594, .T. ) ;
#9547 = CIRCLE ( 'NONE', #15720, 4.000000000000000000 ) ;
#9548 = CARTESIAN_POINT ( 'NONE',  ( 11.64218518496999977, -8.036653071258001546, -4.231765345051999638 ) ) ;
#9549 = CARTESIAN_POINT ( 'NONE',  ( 24.49999999999999645, 1.330573465229666574, 10.33004493691498560 ) ) ;
#9550 = CARTESIAN_POINT ( 'NONE',  ( -4.663699493647997407, 12.43415402266998981, 1.065227872551999466 ) ) ;
#9551 = AXIS2_PLACEMENT_3D ( 'NONE', #13301, #17061, #20700 ) ;
#9552 = CARTESIAN_POINT ( 'NONE',  ( 2.159136702051380308, 29.00043188692588103, 0.05903435693729322531 ) ) ;
#9553 = CARTESIAN_POINT ( 'NONE',  ( -24.46239300412999640, -6.744405939805999672, -8.905960738907999996 ) ) ;
#9554 = EDGE_LOOP ( 'NONE', ( #10911, #11379, #3937, #23562 ) ) ;
#9555 = CIRCLE ( 'NONE', #15733, 2.649999999999999911 ) ;
#9556 = LINE ( 'NONE', #2282, #11144 ) ;
#9557 = EDGE_LOOP ( 'NONE', ( #15386, #17619, #5529, #18525, #23281, #677, #21990, #5313 ) ) ;
#9558 = CARTESIAN_POINT ( 'NONE',  ( -23.50032910583999879, 1.715543117993999783E-14, -9.274346474607714441 ) ) ;
#9559 = CARTESIAN_POINT ( 'NONE',  ( 0.3985328791175999918, 26.31299822781000231, 2.231710853292999897 ) ) ;
#9560 = DIRECTION ( 'NONE',  ( 0.000000000000000000, 1.000000000000000000, 0.000000000000000000 ) ) ;
#9561 = CARTESIAN_POINT ( 'NONE',  ( 0.000000000000000000, -1.550000000000000044, 0.000000000000000000 ) ) ;
#9562 = CARTESIAN_POINT ( 'NONE',  ( 12.56850174931000019, 2.370728120151999629, -10.36336111974000040 ) ) ;
#9563 = CARTESIAN_POINT ( 'NONE',  ( -13.19880458549999958, -0.9434914505904000714, -10.69878979702999899 ) ) ;
#9564 = B_SPLINE_CURVE_WITH_KNOTS ( 'NONE', 3,
 ( #15299, #8296, #15183, #6100, #13732, #11810, #21007, #15544, #10110, #7932 ),
 .UNSPECIFIED., .F., .F.,
 ( 4, 1, 1, 2, 2, 4 ),
 ( 0.000000000000000000, 0.2499999999999994449, 0.3749999999999990563, 0.4374999999999988898, 0.4999999999999987788, 1.000000000000000000 ),
 .UNSPECIFIED. ) ;
#9565 = DIRECTION ( 'NONE',  ( 0.000000000000000000, -1.000000000000000000, 0.000000000000000000 ) ) ;
#9566 = CARTESIAN_POINT ( 'NONE',  ( -14.39391695410597549, -4.126581034250158098, 12.49998949084259614 ) ) ;
#9567 = EDGE_LOOP ( 'NONE', ( #22373, #19532, #10773 ) ) ;
#9568 = CIRCLE ( 'NONE', #6479, 4.750000000000000000 ) ;
#9569 = CARTESIAN_POINT ( 'NONE',  ( -1.497233415519999999, 25.19883331122000314, 2.033913964766000060 ) ) ;
#9570 = CARTESIAN_POINT ( 'NONE',  ( 13.84538782162042381, -8.680617797995118679, 5.551030475077797455 ) ) ;
#9571 = CARTESIAN_POINT ( 'NONE',  ( -24.50000000000000000, 1.524685264937999788E-14, 0.000000000000000000 ) ) ;
#9572 = CARTESIAN_POINT ( 'NONE',  ( 23.50140112429999917, -0.2660373876970000273, -11.28442596635000150 ) ) ;
#9573 = CARTESIAN_POINT ( 'NONE',  ( 2.408588448076999899, 28.72267442561999928, -0.8468005884097000724 ) ) ;
#9574 = ADVANCED_FACE ( 'NONE', ( #8546 ), #12357, .F. ) ;
#9575 = CARTESIAN_POINT ( 'NONE',  ( 11.06619116163201788, -0.4983756420194491166, 12.49999828234741450 ) ) ;
#9576 = CARTESIAN_POINT ( 'NONE',  ( 18.74098996950760565, 2.121065158271645323, 10.25986587397817118 ) ) ;
#9577 = DIRECTION ( 'NONE',  ( 0.000000000000000000, -1.000000000000000000, 0.000000000000000000 ) ) ;
#9578 = CARTESIAN_POINT ( 'NONE',  ( -2.500000000000000888, 29.81753006952333251, -0.3272492347489316944 ) ) ;
#9579 = EDGE_LOOP ( 'NONE', ( #7602, #4194, #23764, #17067 ) ) ;
#9580 = CARTESIAN_POINT ( 'NONE',  ( -14.48343131230104497, 2.223754299675648305, -8.788885103986384451 ) ) ;
#9581 = CARTESIAN_POINT ( 'NONE',  ( 11.70388046505397206, -12.85079422505704017, 2.741654745543806726 ) ) ;
#9582 = AXIS2_PLACEMENT_3D ( 'NONE', #2965, #887, #8290 ) ;
#9583 = EDGE_LOOP ( 'NONE', ( #8214, #12439, #17420, #15535 ) ) ;
#9584 = PRODUCT_DEFINITION_SHAPE ( 'NONE', 'NONE',  #23974 ) ;
#9585 = CARTESIAN_POINT ( 'NONE',  ( 0.000000000000000000, 19.09999999999999787, 0.000000000000000000 ) ) ;
#9586 = LINE ( 'NONE', #13214, #3854 ) ;
#9587 = CARTESIAN_POINT ( 'NONE',  ( -0.7783053373570000266, 28.00000000000000000, 6.000000000000000000 ) ) ;
#9588 = ORIENTED_EDGE ( 'NONE', *, *, #9614, .T. ) ;
#9589 = CARTESIAN_POINT ( 'NONE',  ( 15.92243887344999997, -6.551683564218000022, -8.903917471378999693 ) ) ;
#9590 = LINE ( 'NONE', #7657, #5199 ) ;
#9591 = CARTESIAN_POINT ( 'NONE',  ( -2.857252503208999705, 27.36169433610000112, -0.2814148094396999866 ) ) ;
#9592 = ORIENTED_EDGE ( 'NONE', *, *, #381, .F. ) ;
#9593 = EDGE_LOOP ( 'NONE', ( #9360, #23423, #18342, #699 ) ) ;
#9594 = CARTESIAN_POINT ( 'NONE',  ( -13.99999999999999645, -0.2128887255028979741, -9.534676919017003982 ) ) ;
#9595 = CARTESIAN_POINT ( 'NONE',  ( -10.09066221169000066, -13.14800539653000122, 8.337798847484000575 ) ) ;
#9596 = CARTESIAN_POINT ( 'NONE',  ( -23.74465998031000069, -6.216878364870000340, -12.50000000000000000 ) ) ;
#9597 = CARTESIAN_POINT ( 'NONE',  ( -18.99854661335000117, 6.966878364870000340, 12.06698729810999993 ) ) ;
#9598 = ORIENTED_EDGE ( 'NONE', *, *, #22219, .T. ) ;
#9599 = CARTESIAN_POINT ( 'NONE',  ( -14.49284522991462509, 10.30702784336665978, 7.147655011474417286 ) ) ;
#9600 = CARTESIAN_POINT ( 'NONE',  ( 21.07774770046331625, 5.661224168628396392, -7.366763267202135701 ) ) ;
#9601 = CARTESIAN_POINT ( 'NONE',  ( 6.142488816234497939, 14.18447672331321741, 0.1076473395637999736 ) ) ;
#9602 = CARTESIAN_POINT ( 'NONE',  ( 15.59691868738293863, -7.345342774621501647, 7.289925863788985438 ) ) ;
#9603 = CIRCLE ( 'NONE', #11547, 10.50000000000000000 ) ;
#9604 = CARTESIAN_POINT ( 'NONE',  ( -14.43819794762999997, 5.126061982986000132, 9.736209624113000061 ) ) ;
#9605 = CARTESIAN_POINT ( 'NONE',  ( -2.190643450555000094, 29.98311359149999689, -0.09517956215792000574 ) ) ;
#9606 = CARTESIAN_POINT ( 'NONE',  ( -18.48019363270999804, 4.914628609928000103, -9.714689191606000307 ) ) ;
#9607 = CARTESIAN_POINT ( 'NONE',  ( 1.207017934462505604, 29.67927007522607497, 1.791127842952921823 ) ) ;
#9608 = ORIENTED_EDGE ( 'NONE', *, *, #511, .T. ) ;
#9609 = CARTESIAN_POINT ( 'NONE',  ( -2.157700896676000291, 23.85153623465999928, 0.3212303798653999842 ) ) ;
#9610 = DIRECTION ( 'NONE',  ( 0.000000000000000000, 0.9925668416490733836, -0.1217007183987966479 ) ) ;
#9611 = CARTESIAN_POINT ( 'NONE',  ( -19.55887123173999953, -9.833822427806001798, 3.504477313184999776 ) ) ;
#9612 = CIRCLE ( 'NONE', #4200, 2.729128784747790970 ) ;
#9613 = EDGE_LOOP ( 'NONE', ( #3765, #23411, #21758, #18267, #4918, #21255, #19248 ) ) ;
#9614 = EDGE_CURVE ( 'NONE', #19902, #5259, #757, .T. ) ;
#9615 = FACE_OUTER_BOUND ( 'NONE', #20049, .T. ) ;
#9616 = CARTESIAN_POINT ( 'NONE',  ( 6.642812809165002719, 13.49906599351999859, -0.0001514643891326998028 ) ) ;
#9617 = AXIS2_PLACEMENT_3D ( 'NONE', #5368, #3327, #23656 ) ;
#9618 = DIRECTION ( 'NONE',  ( 0.000000000000000000, 1.000000000000000000, 0.000000000000000000 ) ) ;
#9619 = CARTESIAN_POINT ( 'NONE',  ( 15.34106375730999972, -1.677480367812999917, -9.021981177529999840 ) ) ;
#9620 = VERTEX_POINT ( 'NONE', #20513 ) ;
#9621 = CARTESIAN_POINT ( 'NONE',  ( -6.068436532072000844, 15.62980265433002458, -1.260321238843998604 ) ) ;
#9622 = CARTESIAN_POINT ( 'NONE',  ( -11.00000000000000000, -10.50000000000000000, 0.000000000000000000 ) ) ;
#9623 = CIRCLE ( 'NONE', #18906, 7.100000000000000533 ) ;
#9624 = ORIENTED_EDGE ( 'NONE', *, *, #16075, .F. ) ;
#9625 = CARTESIAN_POINT ( 'NONE',  ( -14.25699038479000080, 13.93375672974000068, -0.1445849984294000079 ) ) ;
#9626 = CARTESIAN_POINT ( 'NONE',  ( 21.92720833333332564, -9.233977095127203327, 1.208851722883240276 ) ) ;
#9627 = CARTESIAN_POINT ( 'NONE',  ( -4.739674965276999608, 12.61450277301999456, -0.05987925791641996592 ) ) ;
#9628 = AXIS2_PLACEMENT_3D ( 'NONE', #12206, #12329, #14015 ) ;
#9629 = CARTESIAN_POINT ( 'NONE',  ( -20.20946649501000181, -9.083415843844999671, 0.0004049750149795999896 ) ) ;
#9630 = CARTESIAN_POINT ( 'NONE',  ( 18.92362270046332640, -4.611705506703642321, -8.001125271793704030 ) ) ;
#9631 = CLOSED_SHELL ( 'NONE', ( #13681, #16223, #1242, #6000, #14287, #21805, #3948, #8508, #1512, #15410, #14149, #22361, #378, #10395, #23451, #8336, #4156, #17570, #6731, #7270, #4366, #3813, #16940, #22106, #16000, #9223, #12105, #17701, #19642, #18796, #11907, #15727, #665, #3787, #23133, #10221, #11046, #4592, #17519, #17224, #21694, #5824, #6230, #19926, #18440, #19267, #20201, #8229, #5813, #11441, #7123, #21864, #10366, #7030, #18278, #23324, #14797, #14852, #23630, #18986, #17525, #15318, #22880, #12960, #8063, #20383, #23309, #13804, #10708, #21925, #17045, #9415, #69, #9662, #8862, #14851, #22423, #19605, #13994, #15934, #16795, #19611, #21085, #21338, #2857, #19118, #17089, #17379, #14076, #5333, #18971, #12200, #5084, #23389, #20491, #5252, #18665, #450, #4288, #1214, #3434, #9255, #9939, #16809, #17796, #22569, #13421, #3487, #1858, #7799, #21409, #16485, #10871, #22414, #8241, #12947, #13503, #16675, #16, #11007, #18297, #14559, #8478, #20663, #21217, #11308, #1027, #17239, #17697, #4080, #11016, #16582, #11788, #18308, #15707, #18425, #3484, #8450, #23870, #12678, #5293, #9574, #16028, #13099, #778, #7938, #16044, #8786, #18593, #943, #21114, #15896, #2162, #18807, #21698, #5072, #5963, #15117, #16633, #20338, #12388, #4067, #10591, #18591, #18083, #7300, #20080, #13133, #22984, #23499, #2585, #10848, #5655, #9955, #19593, #4793, #22640, #11266, #2691 ) ) ;
#9632 = CARTESIAN_POINT ( 'NONE',  ( -6.250000000000000000, 16.31160201366999729, -1.000000000001000089 ) ) ;
#9633 = CARTESIAN_POINT ( 'NONE',  ( 13.50000000000000000, 0.000000000000000000, 0.000000000000000000 ) ) ;
#9634 = AXIS2_PLACEMENT_3D ( 'NONE', #19872, #19515, #12374 ) ;
#9635 = CARTESIAN_POINT ( 'NONE',  ( 0.9744765624120645953, 26.41693820796410819, -4.056187847889995979 ) ) ;
#9636 = DIRECTION ( 'NONE',  ( -0.7071067811865465735, -0.7071067811865465735, -5.144932280347337440E-08 ) ) ;
#9637 = CARTESIAN_POINT ( 'NONE',  ( 2.142844928456669962, 30.58794887508146232, 0.2701627623478729534 ) ) ;
#9638 = ORIENTED_EDGE ( 'NONE', *, *, #9413, .F. ) ;
#9639 = CARTESIAN_POINT ( 'NONE',  ( 22.73928674176000087, -5.367530796503000801, -8.899542937657001218 ) ) ;
#9640 = CARTESIAN_POINT ( 'NONE',  ( 3.249297074264064555, 13.15931643686085728, -5.930092486474230817 ) ) ;
#9641 = DIRECTION ( 'NONE',  ( 0.000000000000000000, 0.000000000000000000, -1.000000000000000000 ) ) ;
#9642 = AXIS2_PLACEMENT_3D ( 'NONE', #16915, #18975, #20799 ) ;
#9643 = EDGE_CURVE ( 'NONE', #9739, #11734, #3459, .T. ) ;
#9644 = CARTESIAN_POINT ( 'NONE',  ( -21.39401291616239931, -4.743783438882505976, 9.554723409011961266 ) ) ;
#9645 = CARTESIAN_POINT ( 'NONE',  ( 0.4330518317348999724, 26.24446440326000030, 2.425010641684000046 ) ) ;
#9646 = AXIS2_PLACEMENT_3D ( 'NONE', #1054, #4578, #11969 ) ;
#9647 = AXIS2_PLACEMENT_3D ( 'NONE', #15729, #15968, #23117 ) ;
#9648 = CARTESIAN_POINT ( 'NONE',  ( -4.000000000000000000, 24.80000000000000426, -2.309401076759000304 ) ) ;
#9649 = ORIENTED_EDGE ( 'NONE', *, *, #9682, .T. ) ;
#9650 = DIRECTION ( 'NONE',  ( 0.000000000000000000, 0.000000000000000000, -1.000000000000000000 ) ) ;
#9651 = CARTESIAN_POINT ( 'NONE',  ( -24.12232999016000079, -13.23032192315998401, 0.000000000000000000 ) ) ;
#9652 = CARTESIAN_POINT ( 'NONE',  ( 2.169463140925995237, 28.02568812777378326, 0.06845542556112334254 ) ) ;
#9653 = DIRECTION ( 'NONE',  ( 1.000000000000000000, 0.000000000000000000, 0.000000000000000000 ) ) ;
#9654 = EDGE_CURVE ( 'NONE', #20433, #22434, #19251, .T. ) ;
#9655 = EDGE_LOOP ( 'NONE', ( #1845, #21981, #4503, #11895, #17680 ) ) ;
#9656 = DIRECTION ( 'NONE',  ( 0.000000000000000000, 0.000000000000000000, 1.000000000000000000 ) ) ;
#9657 = CARTESIAN_POINT ( 'NONE',  ( 18.71100174931000026, 5.082731606397000057, 9.520742961040999930 ) ) ;
#9658 = CARTESIAN_POINT ( 'NONE',  ( -16.78192513375999795, 10.68652398881999943, -3.898064904104000306 ) ) ;
#9659 = CARTESIAN_POINT ( 'NONE',  ( 23.96190874292139128, -7.512837009555735968, -5.581780844827100907 ) ) ;
#9660 = CARTESIAN_POINT ( 'NONE',  ( 19.39051537306000128, -5.800580820157000161, 8.214924713229001085 ) ) ;
#9661 = CARTESIAN_POINT ( 'NONE',  ( 4.750000000000000000, 21.89999999999999858, 0.000000000000000000 ) ) ;
#9662 = ADVANCED_FACE ( 'NONE', ( #18574, #15485 ), #19249, .F. ) ;
#9663 = LINE ( 'NONE', #441, #3695 ) ;
#9664 = CARTESIAN_POINT ( 'NONE',  ( 20.66721036671000178, 8.339588664129999884, -5.894560743941999803 ) ) ;
#9665 = CARTESIAN_POINT ( 'NONE',  ( 24.48327518124252933, -10.18191985984368664, 7.364397484155817963 ) ) ;
#9666 = EDGE_LOOP ( 'NONE', ( #18641, #5284, #1614, #11116 ) ) ;
#9667 = FACE_OUTER_BOUND ( 'NONE', #16551, .T. ) ;
#9668 = CARTESIAN_POINT ( 'NONE',  ( -2.607696352436000176, 26.38206776952000254, 0.5721489135198000175 ) ) ;
#9669 = AXIS2_PLACEMENT_3D ( 'NONE', #22342, #2124, #3950 ) ;
#9670 = CARTESIAN_POINT ( 'NONE',  ( 4.913522824441004744, 12.43887836712999473, 0.2526796349711001310 ) ) ;
#9671 = CARTESIAN_POINT ( 'NONE',  ( 0.000000000000000000, 27.25000000000000000, 0.000000000000000000 ) ) ;
#9672 = EDGE_CURVE ( 'NONE', #13697, #12220, #3942, .T. ) ;
#9673 = CARTESIAN_POINT ( 'NONE',  ( -24.62947754991999716, -9.950913960798999369, -3.563496608132999732 ) ) ;
#9674 = ORIENTED_EDGE ( 'NONE', *, *, #21792, .F. ) ;
#9675 = CARTESIAN_POINT ( 'NONE',  ( -20.44776253787999920, -9.196011600180998613, 0.000000000000000000 ) ) ;
#9676 = EDGE_LOOP ( 'NONE', ( #823, #5843, #7689, #12114 ) ) ;
#9677 = CYLINDRICAL_SURFACE ( 'NONE', #3727, 10.59999999999999964 ) ;
#9678 = DIRECTION ( 'NONE',  ( -1.000000000000000000, 0.000000000000000000, 0.000000000000000000 ) ) ;
#9679 = CARTESIAN_POINT ( 'NONE',  ( 1.403495832404999977, 26.60549822781000273, -1.780325977227999790 ) ) ;
#9680 = CARTESIAN_POINT ( 'NONE',  ( 16.39158103379666187, -1.190002857594419705, 9.091921988472257965 ) ) ;
#9681 = CARTESIAN_POINT ( 'NONE',  ( 14.76225174930999984, 10.68374474379000105, -0.3265774252310000292 ) ) ;
#9682 = EDGE_CURVE ( 'NONE', #19420, #12075, #2519, .T. ) ;
#9683 = CARTESIAN_POINT ( 'NONE',  ( -17.62691415960999919, 5.507581498160999622, 8.736692431694999428 ) ) ;
#9684 = CARTESIAN_POINT ( 'NONE',  ( 18.26606375730999687, -4.551782674040000032, 7.886397731525000232 ) ) ;
#9685 = CARTESIAN_POINT ( 'NONE',  ( 24.32802197706137903, 12.60002805950083982, -3.176111224150924173 ) ) ;
#9686 = ORIENTED_EDGE ( 'NONE', *, *, #16764, .T. ) ;
#9687 = CARTESIAN_POINT ( 'NONE',  ( 0.000000000000000000, 29.84999999328000087, 0.000000000000000000 ) ) ;
#9688 = CARTESIAN_POINT ( 'NONE',  ( 2.411685057264000065, 23.91801102320000183, -0.7498601224302000601 ) ) ;
#9689 = CARTESIAN_POINT ( 'NONE',  ( 13.84536273287771202, -8.680155482951017021, 5.551750670585463787 ) ) ;
#9690 = ORIENTED_EDGE ( 'NONE', *, *, #21060, .T. ) ;
#9691 = DIRECTION ( 'NONE',  ( -1.000000000000000000, 0.000000000000000000, 0.000000000000000000 ) ) ;
#9692 =( NAMED_UNIT ( * ) SI_UNIT ( $, .STERADIAN. ) SOLID_ANGLE_UNIT ( ) );
#9693 = CARTESIAN_POINT ( 'NONE',  ( -2.375794074296999625, 30.62788859182999701, 1.065851494486000028 ) ) ;
#9694 = CARTESIAN_POINT ( 'NONE',  ( 11.78924557931383177, 4.312980057964804104, 12.49999285599082377 ) ) ;
#9695 = CARTESIAN_POINT ( 'NONE',  ( 13.50000000000000000, -10.65000000000000036, 0.000000000000000000 ) ) ;
#9696 = CARTESIAN_POINT ( 'NONE',  ( -6.694406957049796603, 15.35878686133300342, 1.695873640511939007 ) ) ;
#9697 = EDGE_CURVE ( 'NONE', #7168, #14405, #9623, .T. ) ;
#9698 = CARTESIAN_POINT ( 'NONE',  ( 12.28022044529580015, 7.993836135665516096, -11.15426966564930744 ) ) ;
#9699 = VERTEX_POINT ( 'NONE', #4728 ) ;
#9700 = EDGE_CURVE ( 'NONE', #11090, #4666, #16212, .T. ) ;
#9701 = DIRECTION ( 'NONE',  ( 1.000000000000000000, 0.000000000000000000, 0.000000000000000000 ) ) ;
#9702 = VERTEX_POINT ( 'NONE', #19747 ) ;
#9703 = CARTESIAN_POINT ( 'NONE',  ( -0.04686596309914999731, 25.05782222538000070, 2.736742389782000018 ) ) ;
#9705 = CARTESIAN_POINT ( 'NONE',  ( -2.163337044627856365, 24.58232107606292516, -0.3658931050139514474 ) ) ;
#9704 = FACE_OUTER_BOUND ( 'NONE', #9211, .T. ) ;
#9706 = CARTESIAN_POINT ( 'NONE',  ( 0.000000000000000000, 15.44510233504000141, 0.000000000000000000 ) ) ;
#9707 = ORIENTED_EDGE ( 'NONE', *, *, #12067, .F. ) ;
#9708 = CARTESIAN_POINT ( 'NONE',  ( 6.159666495275548215, 14.07295743052582360, -0.4000666433572926395 ) ) ;
#9709 = CONICAL_SURFACE ( 'NONE', #18600, 4.674999979945999584, 0.7853981633972997312 ) ;
#9710 = CARTESIAN_POINT ( 'NONE',  ( 0.000000000000000000, 16.95000012746599793, -2.704938617610999654E-14 ) ) ;
#9711 = CARTESIAN_POINT ( 'NONE',  ( -1.948889566018999986, 26.67919433610000013, 2.108296854627000005 ) ) ;
#9712 = EDGE_CURVE ( 'NONE', #14929, #7412, #8598, .T. ) ;
#9713 = EDGE_LOOP ( 'NONE', ( #13322, #23821, #16925, #5837, #19940, #23278, #6914, #11916, #22430 ) ) ;
#9714 = ORIENTED_EDGE ( 'NONE', *, *, #14150, .F. ) ;
#9715 = EDGE_CURVE ( 'NONE', #13716, #23321, #13498, .T. ) ;
#9716 = CARTESIAN_POINT ( 'NONE',  ( -14.00000000000000000, -5.610885045639453672, -8.079343806354058799 ) ) ;
#9717 = CARTESIAN_POINT ( 'NONE',  ( -10.80341971169000104, 14.28377837372999970, -6.193755811534000344 ) ) ;
#9718 = CARTESIAN_POINT ( 'NONE',  ( 0.000000000000000000, 0.000000000000000000, 0.000000000000000000 ) ) ;
#9719 = LINE ( 'NONE', #9834, #508 ) ;
#9720 = VERTEX_POINT ( 'NONE', #17925 ) ;
#9721 = CARTESIAN_POINT ( 'NONE',  ( -21.65907966340000002, 3.174516240292999836, -9.136279537863000400 ) ) ;
#9722 = CARTESIAN_POINT ( 'NONE',  ( -14.25243324638999809, 7.716878364870000340, 11.63397459621999985 ) ) ;
#9723 = CARTESIAN_POINT ( 'NONE',  ( 6.158244933928628484, 14.08141442615745653, 0.3795422047411434185 ) ) ;
#9724 = CARTESIAN_POINT ( 'NONE',  ( 15.27210601666787149, 3.430796689683968559, 9.762251594826194534 ) ) ;
#9725 = CARTESIAN_POINT ( 'NONE',  ( 0.000000000000000000, 28.00000000000000000, 0.000000000000000000 ) ) ;
#9726 = CARTESIAN_POINT ( 'NONE',  ( 0.3249195791085000007, 29.65169427534999969, 2.164038618295999861 ) ) ;
#9727 = CARTESIAN_POINT ( 'NONE',  ( -17.87080258880000017, 5.796842063356000274, 9.195416763971000051 ) ) ;
#9728 = CARTESIAN_POINT ( 'NONE',  ( 0.4950218517047121902, 29.63316247012222604, 2.102426574152561400 ) ) ;
#9729 = VERTEX_POINT ( 'NONE', #3032 ) ;
#9730 = B_SPLINE_CURVE_WITH_KNOTS ( 'NONE', 3,
 ( #19563, #774, #1017, #6226, #12173, #12054, #10230, #23049, #8175, #17498 ),
 .UNSPECIFIED., .F., .F.,
 ( 4, 2, 2, 2, 4 ),
 ( 0.000000000000000000, 0.06692748465457198925, 0.1338549693091439785, 0.2007824539637159678, 0.2677099386182879570 ),
 .UNSPECIFIED. ) ;
#9731 = CARTESIAN_POINT ( 'NONE',  ( -1.974988437399999963, 24.44503257140999963, 0.9367674359008000273 ) ) ;
#9732 = CARTESIAN_POINT ( 'NONE',  ( -19.38267422463178491, -10.23251295633816227, -2.712185686795678397 ) ) ;
#9733 = APPLICATION_CONTEXT ( 'automotive_design' ) ;
#9734 = VERTEX_POINT ( 'NONE', #1330 ) ;
#9735 = DIRECTION ( 'NONE',  ( 0.000000000000000000, -1.000000000000000000, 0.000000000000000000 ) ) ;
#9736 = CARTESIAN_POINT ( 'NONE',  ( -4.941117876443001933, 15.61713999035001343, 3.125961572582002024 ) ) ;
#9737 = CARTESIAN_POINT ( 'NONE',  ( 18.26141666666665131, -8.901969795568348331, 2.392468253058787298 ) ) ;
#9738 = CARTESIAN_POINT ( 'NONE',  ( 12.62531392131000096, 8.177682633693001080, 5.055777280222000236 ) ) ;
#9739 = VERTEX_POINT ( 'NONE', #8719 ) ;
#9740 = CARTESIAN_POINT ( 'NONE',  ( -6.228095582201001790, 16.43254147212998362, -1.007191989855000358 ) ) ;
#9741 = LINE ( 'NONE', #13252, #7580 ) ;
#9742 = CIRCLE ( 'NONE', #18263, 2.999999999999999556 ) ;
#9743 = ORIENTED_EDGE ( 'NONE', *, *, #12365, .F. ) ;
#9744 = DIRECTION ( 'NONE',  ( 0.000000000000000000, 0.000000000000000000, 1.000000000000000000 ) ) ;
#9745 = CARTESIAN_POINT ( 'NONE',  ( -11.62500000000000000, 1.367011989547999955E-14, 0.000000000000000000 ) ) ;
#9746 = CARTESIAN_POINT ( 'NONE',  ( -3.142350709629999628, 12.07584853453000129, 3.567860278848001165 ) ) ;
#9747 = DIRECTION ( 'NONE',  ( 1.000000000000000000, 0.000000000000000000, 0.000000000000000000 ) ) ;
#9748 = CARTESIAN_POINT ( 'NONE',  ( -23.58178687934999829, -6.109693073218999793, -7.476155833321000088 ) ) ;
#9749 = DIRECTION ( 'NONE',  ( -1.000000000000000000, 0.000000000000000000, 0.000000000000000000 ) ) ;
#9750 = CARTESIAN_POINT ( 'NONE',  ( -4.628018178257720550, 13.45824813671923437, 5.216489783566583327 ) ) ;
#9751 = DIRECTION ( 'NONE',  ( -1.000000000000000000, 0.000000000000000000, 0.000000000000000000 ) ) ;
#9752 = CARTESIAN_POINT ( 'NONE',  ( 5.048072026126640743, 14.71121043296684761, 3.475281950094643690 ) ) ;
#9753 = CARTESIAN_POINT ( 'NONE',  ( -0.7783053373570000266, 26.50000000000000000, 6.000000000000000000 ) ) ;
#9754 = CARTESIAN_POINT ( 'NONE',  ( 0.3916584102265154854, 30.42698342189353866, 2.124085250123096902 ) ) ;
#9755 = ORIENTED_EDGE ( 'NONE', *, *, #20221, .F. ) ;
#9756 = FACE_OUTER_BOUND ( 'NONE', #23874, .T. ) ;
#9757 = CARTESIAN_POINT ( 'NONE',  ( 3.630616870732635615, 13.24606289761949007, -5.733978109788271382 ) ) ;
#9758 = CARTESIAN_POINT ( 'NONE',  ( -23.60559742078757139, -8.658706366674554289, -3.691114709487112844 ) ) ;
#9759 = CARTESIAN_POINT ( 'NONE',  ( -22.30440966686241566, 4.682851881239854741, -9.610650805105821703 ) ) ;
#9760 = CARTESIAN_POINT ( 'NONE',  ( -2.288454502553999959, 26.79614211382000022, 0.1349572241793000060 ) ) ;
#9761 = CONICAL_SURFACE ( 'NONE', #18652, 4.309401076758999416, 1.119376321708719590 ) ;
#9762 = CARTESIAN_POINT ( 'NONE',  ( 1.709999999999999964, 9.000000000000000000, 0.3720215047547999476 ) ) ;
#9763 = ORIENTED_EDGE ( 'NONE', *, *, #22703, .F. ) ;
#9764 = DIRECTION ( 'NONE',  ( 0.000000000000000000, 0.000000000000000000, 1.000000000000000000 ) ) ;
#9765 = CARTESIAN_POINT ( 'NONE',  ( 24.32771143580656314, 9.033746532951345998, -3.774273071546123681 ) ) ;
#9766 = EDGE_CURVE ( 'NONE', #8792, #18916, #23883, .T. ) ;
#9767 = CARTESIAN_POINT ( 'NONE',  ( 1.359641396650144607, 27.91473787195837275, 1.732418534185389047 ) ) ;
#9768 = ORIENTED_EDGE ( 'NONE', *, *, #805, .F. ) ;
#9769 = ORIENTED_EDGE ( 'NONE', *, *, #22866, .F. ) ;
#9770 = DIRECTION ( 'NONE',  ( 1.000000000000000000, 0.000000000000000000, 0.000000000000000000 ) ) ;
#9771 = CARTESIAN_POINT ( 'NONE',  ( 16.29787674931000296, 5.844090361140000134, -8.997790218903000792 ) ) ;
#9772 = EDGE_CURVE ( 'NONE', #2323, #10715, #3855, .T. ) ;
#9773 = CARTESIAN_POINT ( 'NONE',  ( -14.34436095811999934, -2.679964408802999909, 10.98515472083999889 ) ) ;
#9774 = CARTESIAN_POINT ( 'NONE',  ( -10.04561490872999840, 16.32684872326999681, 0.9999999999983000265 ) ) ;
#9775 = CARTESIAN_POINT ( 'NONE',  ( 19.66181994525999954, -5.517917554610000330, 7.814610069288999483 ) ) ;
#9776 = CARTESIAN_POINT ( 'NONE',  ( 13.50000000000000178, -7.092774689729933080, -5.968849012436532320 ) ) ;
#9777 = AXIS2_PLACEMENT_3D ( 'NONE', #10083, #10328, #4639 ) ;
#9778 = CARTESIAN_POINT ( 'NONE',  ( 2.184465970885649089, 26.96753006952332399, 1.259047450927240241 ) ) ;
#9779 = CARTESIAN_POINT ( 'NONE',  ( 22.53195685829999917, 1.853256702191000027, -9.556221255016000171 ) ) ;
#9780 = CARTESIAN_POINT ( 'NONE',  ( 0.000000000000000000, 15.05000017415440006, 0.000000000000000000 ) ) ;
#9781 = ORIENTED_EDGE ( 'NONE', *, *, #1541, .T. ) ;
#9782 = CARTESIAN_POINT ( 'NONE',  ( 0.000000000000000000, 16.95000012746599793, 0.000000000000000000 ) ) ;
#9783 = CARTESIAN_POINT ( 'NONE',  ( 2.628147087956000050, 28.33206776952000183, 0.4693273880717999669 ) ) ;
#9784 = CARTESIAN_POINT ( 'NONE',  ( -1.066174337946000250, 11.54162544571998872, 4.691709464589000511 ) ) ;
#9785 = CARTESIAN_POINT ( 'NONE',  ( 2.091722048788486887, 29.03591149769223989, -0.5394191446943552570 ) ) ;
#9786 = EDGE_CURVE ( 'NONE', #17452, #7412, #14066, .T. ) ;
#9787 = CARTESIAN_POINT ( 'NONE',  ( -22.77108459744000157, -5.959070222075999901, -9.395571579996001788 ) ) ;
#9788 = EDGE_LOOP ( 'NONE', ( #13249, #5591 ) ) ;
#9789 = DIRECTION ( 'NONE',  ( -1.000000000000000000, 0.000000000000000000, 0.000000000000000000 ) ) ;
#9790 = VERTEX_POINT ( 'NONE', #23953 ) ;
#9791 = CARTESIAN_POINT ( 'NONE',  ( -23.86847083088467869, 5.679235826614652538, -12.50000000000279599 ) ) ;
#9792 = CARTESIAN_POINT ( 'NONE',  ( 0.000000000000000000, 14.95000002005000006, 0.000000000000000000 ) ) ;
#9793 = CARTESIAN_POINT ( 'NONE',  ( 0.5289967318967999654, 28.15756359723999935, -2.411020654974999733 ) ) ;
#9794 = CARTESIAN_POINT ( 'NONE',  ( 16.80728936713000365, -9.102589883624000677, 0.000000000000000000 ) ) ;
#9795 =( GEOMETRIC_REPRESENTATION_CONTEXT ( 3 ) GLOBAL_UNCERTAINTY_ASSIGNED_CONTEXT ( ( #22026 ) ) GLOBAL_UNIT_ASSIGNED_CONTEXT ( ( #6673, #6921, #23633 ) ) REPRESENTATION_CONTEXT ( 'NONE', 'WORKASPACE' ) );
#9796 = CARTESIAN_POINT ( 'NONE',  ( -1.158286564292558829, 6.875900300209513816, 1.312442925060462562 ) ) ;
#9797 = CARTESIAN_POINT ( 'NONE',  ( 13.66537674931000090, -8.233391669162999804, 6.770876163316000174 ) ) ;
#9798 = CARTESIAN_POINT ( 'NONE',  ( -14.17369824411999879, 9.412195986946999327, 4.011894131497999005 ) ) ;
#9799 = CARTESIAN_POINT ( 'NONE',  ( 18.19293875730999943, -2.463108239980999592, 8.917637382198998708 ) ) ;
#9800 = AXIS2_PLACEMENT_3D ( 'NONE', #13947, #5006, #12393 ) ;
#9801 = CARTESIAN_POINT ( 'NONE',  ( -14.47125380616081181, 2.070155988425159244, 12.49997628898002944 ) ) ;
#9802 = EDGE_CURVE ( 'NONE', #3210, #2430, #3106, .T. ) ;
#9803 = ORIENTED_EDGE ( 'NONE', *, *, #7098, .T. ) ;
#9804 =( NAMED_UNIT ( * ) PLANE_ANGLE_UNIT ( ) SI_UNIT ( $, .RADIAN. ) );
#9805 = CARTESIAN_POINT ( 'NONE',  ( 2.480184517804000066, 25.41360425264999634, -0.7931718914648999696 ) ) ;
#9806 = CARTESIAN_POINT ( 'NONE',  ( 14.23170285492579801, -7.372315516923570122, -7.223174187050277695 ) ) ;
#9807 = ORIENTED_EDGE ( 'NONE', *, *, #16810, .T. ) ;
#9808 = CARTESIAN_POINT ( 'NONE',  ( 4.833250487806001416, 14.92157114608998469, -3.774880232157002524 ) ) ;
#9809 = DIRECTION ( 'NONE',  ( 0.000000000000000000, 0.000000000000000000, 1.000000000000000000 ) ) ;
#9810 = DIRECTION ( 'NONE',  ( -1.000000000000000000, 0.000000000000000000, 0.000000000000000000 ) ) ;
#9811 = CARTESIAN_POINT ( 'NONE',  ( 14.39275807839523580, -4.136262847370294260, 8.039618612950896193 ) ) ;
#9812 = CARTESIAN_POINT ( 'NONE',  ( 17.98830562607077965, 3.393379461346332171, -9.888719939816333238 ) ) ;
#9813 = CARTESIAN_POINT ( 'NONE',  ( 12.00000000000000000, 0.000000000000000000, 1.045589212608000028E-14 ) ) ;
#9814 = CARTESIAN_POINT ( 'NONE',  ( -2.399999999999999911, 30.00000000000000000, 0.000000000000000000 ) ) ;
#9815 = VECTOR ( 'NONE', #736, 1000.000000000000114 ) ;
#9816 = EDGE_CURVE ( 'NONE', #4661, #22477, #7013, .T. ) ;
#9817 = CARTESIAN_POINT ( 'NONE',  ( -2.500000000000000000, 29.83419673618999823, 0.000000000000000000 ) ) ;
#9818 = VERTEX_POINT ( 'NONE', #20323 ) ;
#9819 = DIRECTION ( 'NONE',  ( -1.000000000000000000, 0.000000000000000000, 0.000000000000000000 ) ) ;
#9820 = VERTEX_POINT ( 'NONE', #11121 ) ;
#9821 = LINE ( 'NONE', #13688, #23454 ) ;
#9823 = CARTESIAN_POINT ( 'NONE',  ( -2.128189877949903774, 23.77262414965302284, -0.5291991134722092704 ) ) ;
#9822 = CARTESIAN_POINT ( 'NONE',  ( -3.055307665906170644, 11.87602316546083969, 3.736655301196532886 ) ) ;
#9824 = DIRECTION ( 'NONE',  ( -0.7071067811823850136, 0.7071067811898851252, -1.080116767747976029E-06 ) ) ;
#9825 = AXIS2_PLACEMENT_3D ( 'NONE', #20356, #21822, #14542 ) ;
#9826 = FACE_OUTER_BOUND ( 'NONE', #8649, .T. ) ;
#9827 = PLANE ( 'NONE',  #17960 ) ;
#9828 = EDGE_CURVE ( 'NONE', #3305, #11676, #23937, .T. ) ;
#9829 = DIRECTION ( 'NONE',  ( 0.000000000000000000, -0.7071067811866525998, -0.7071067811864425456 ) ) ;
#9830 = ORIENTED_EDGE ( 'NONE', *, *, #15760, .F. ) ;
#9831 = VERTEX_POINT ( 'NONE', #20213 ) ;
#9832 = CARTESIAN_POINT ( 'NONE',  ( -24.47970833437427984, 10.31330985778130227, -7.136763535915959800 ) ) ;
#9833 = CARTESIAN_POINT ( 'NONE',  ( 2.900806500513820829, 29.93562577624027909, -2.944020739578861789 ) ) ;
#9834 = CARTESIAN_POINT ( 'NONE',  ( -4.549999861571000004, 21.99999986157541798, 6.289351259589999728E-08 ) ) ;
#9835 = EDGE_CURVE ( 'NONE', #22702, #3216, #3079, .T. ) ;
#9836 = ORIENTED_EDGE ( 'NONE', *, *, #12795, .T. ) ;
#9837 = CARTESIAN_POINT ( 'NONE',  ( -22.07433482820000137, -2.615545669082999680, -9.865490644338999360 ) ) ;
#9838 = ADVANCED_FACE ( 'NONE', ( #14629 ), #21794, .F. ) ;
#9839 = CARTESIAN_POINT ( 'NONE',  ( -24.24003052282993309, 9.030352382186375593, 9.358674018443513987 ) ) ;
#9840 = CARTESIAN_POINT ( 'NONE',  ( 0.000000000000000000, 0.000000000000000000, -7.500000000000000000 ) ) ;
#9841 = CARTESIAN_POINT ( 'NONE',  ( 15.74491607068019938, -9.964074634268969888, 2.836190018388155654 ) ) ;
#9842 = CARTESIAN_POINT ( 'NONE',  ( -19.06736070216000201, 2.265016177855000201, -10.89708866536000009 ) ) ;
#9843 = CARTESIAN_POINT ( 'NONE',  ( 1.691667482778999920, 30.51999502565000100, -1.640128175915999797 ) ) ;
#9844 = CARTESIAN_POINT ( 'NONE',  ( -20.97328328328443092, -5.337166430913867110, -9.061234812632074309 ) ) ;
#9845 = CARTESIAN_POINT ( 'NONE',  ( -18.88645432865000018, -8.793774626762999702, -6.438463651166999924 ) ) ;
#9846 = CARTESIAN_POINT ( 'NONE',  ( -0.04072186729643159642, 29.60146742886088589, 2.159503982503783615 ) ) ;
#9847 = ADVANCED_FACE ( 'NONE', ( #5319 ), #20102, .T. ) ;
#9848 = ORIENTED_EDGE ( 'NONE', *, *, #13460, .F. ) ;
#9849 = CARTESIAN_POINT ( 'NONE',  ( 2.054615896157999888, 24.75754592284000211, 1.138344536031999921 ) ) ;
#9850 = EDGE_CURVE ( 'NONE', #12335, #23570, #18279, .T. ) ;
#9851 = AXIS2_PLACEMENT_3D ( 'NONE', #23753, #19659, #7157 ) ;
#9852 = LINE ( 'NONE', #16869, #10043 ) ;
#9853 = EDGE_LOOP ( 'NONE', ( #18071, #8665, #14904 ) ) ;
#9854 = LINE ( 'NONE', #17484, #11068 ) ;
#9855 = CARTESIAN_POINT ( 'NONE',  ( -4.728521406481004163, 15.35552965760000710, 3.489357254952003551 ) ) ;
#9856 = VECTOR ( 'NONE', #242, 1000.000000000000000 ) ;
#9857 = DIRECTION ( 'NONE',  ( 0.000000000000000000, 1.000000000000000000, 0.000000000000000000 ) ) ;
#9858 = CARTESIAN_POINT ( 'NONE',  ( 14.27062642131000025, 9.653071988928001446, -0.2951073761277999696 ) ) ;
#9859 = ORIENTED_EDGE ( 'NONE', *, *, #14977, .T. ) ;
#9860 = CARTESIAN_POINT ( 'NONE',  ( -6.318227646113002471, 16.43048641157998802, -1.007191989855000358 ) ) ;
#9861 = DIRECTION ( 'NONE',  ( 0.000000000000000000, -1.000000000000000000, 0.000000000000000000 ) ) ;
#9862 = VERTEX_POINT ( 'NONE', #13280 ) ;
#9863 = CARTESIAN_POINT ( 'NONE',  ( 4.000000000000000000, 26.37490599056222962, -1.464369514602714251 ) ) ;
#9864 = CARTESIAN_POINT ( 'NONE',  ( 21.32254166666666606, 5.665264218082834979, 7.371607159753769345 ) ) ;
#9865 = CARTESIAN_POINT ( 'NONE',  ( 24.38244769084932528, -4.973698664748710030, 9.391432790414068421 ) ) ;
#9866 = CARTESIAN_POINT ( 'NONE',  ( -4.649999999999999467, 22.00000000000000000, 0.000000000000000000 ) ) ;
#9867 = CARTESIAN_POINT ( 'NONE',  ( 17.67377246198465812, -10.31525896512351714, -1.350505006071770486 ) ) ;
#9868 = DIRECTION ( 'NONE',  ( 1.000000000000000000, 0.000000000000000000, 0.000000000000000000 ) ) ;
#9869 = CARTESIAN_POINT ( 'NONE',  ( -14.32799115970092174, 8.244301755411150623, -10.71998578050881790 ) ) ;
#9870 = CARTESIAN_POINT ( 'NONE',  ( 23.99062354302999722, -13.93375672974000068, 0.8660254037843999608 ) ) ;
#9871 = DIRECTION ( 'NONE',  ( 0.000000000000000000, -1.000000000000000000, 0.000000000000000000 ) ) ;
#9872 = CARTESIAN_POINT ( 'NONE',  ( 1.350914310362234527, 26.47444252552741872, -3.838851412777818606 ) ) ;
#9873 = CARTESIAN_POINT ( 'NONE',  ( 2.434931691670788823, 27.86753006952332612, -0.6543697108982007293 ) ) ;
#9874 = CARTESIAN_POINT ( 'NONE',  ( 0.3871515648526898112, 30.42671105185918279, 2.124914593381988848 ) ) ;
#9875 = EDGE_CURVE ( 'NONE', #11676, #3528, #22485, .T. ) ;
#9876 = VERTEX_POINT ( 'NONE', #2504 ) ;
#9877 = CARTESIAN_POINT ( 'NONE',  ( 20.17446287504999702, -7.350134498294000451, 6.461420190107999950 ) ) ;
#9878 = CARTESIAN_POINT ( 'NONE',  ( -1.717182781518961976, 12.90331733707204087, -6.468384628374955092 ) ) ;
#9879 = CARTESIAN_POINT ( 'NONE',  ( 1.699999998837999904, 12.90000000000000036, -1.053565373074999867 ) ) ;
#9880 = CARTESIAN_POINT ( 'NONE',  ( -0.7145966149424999303, 28.58446440326000015, 2.357055497444999759 ) ) ;
#9881 = AXIS2_PLACEMENT_3D ( 'NONE', #7643, #19388, #12125 ) ;
#9882 = DIRECTION ( 'NONE',  ( -1.000000000000000000, 0.000000000000000000, 0.000000000000000000 ) ) ;
#9883 = ORIENTED_EDGE ( 'NONE', *, *, #21768, .T. ) ;
#9884 = CARTESIAN_POINT ( 'NONE',  ( -18.91245535748801032, -3.755334353860249497, -9.775979986752766138 ) ) ;
#9885 = CARTESIAN_POINT ( 'NONE',  ( 24.15736593521746300, 13.39690473052857378, 1.795880342563474397 ) ) ;
#9886 = CARTESIAN_POINT ( 'NONE',  ( -1.817280340265412519, 28.50647256964058229, 1.244239457231288926 ) ) ;
#9887 = VERTEX_POINT ( 'NONE', #318 ) ;
#9888 = ORIENTED_EDGE ( 'NONE', *, *, #2144, .T. ) ;
#9889 = CARTESIAN_POINT ( 'NONE',  ( 0.000000000000000000, 16.95000012746599793, 0.000000000000000000 ) ) ;
#9890 = CARTESIAN_POINT ( 'NONE',  ( 18.82068924930999998, 1.189837805593999986, 10.72966125727000097 ) ) ;
#9891 = CARTESIAN_POINT ( 'NONE',  ( -14.23644303527998822, 0.6063593516544601991, -9.063592691554708480 ) ) ;
#9892 = VECTOR ( 'NONE', #18949, 1000.000000000000000 ) ;
#9893 = CARTESIAN_POINT ( 'NONE',  ( 0.000000000000000000, 19.00000000000000000, 0.000000000000000000 ) ) ;
#9894 = CARTESIAN_POINT ( 'NONE',  ( 0.000000000000000000, 18.00000000000000000, 0.000000000000000000 ) ) ;
#9895 = CARTESIAN_POINT ( 'NONE',  ( 16.34364037305999773, -5.328133213713000416, -9.435500363287999903 ) ) ;
#9896 = DIRECTION ( 'NONE',  ( 1.000000000000000000, 0.000000000000000000, 0.000000000000000000 ) ) ;
#9897 = AXIS2_PLACEMENT_3D ( 'NONE', #12937, #20567, #18746 ) ;
#9898 = CARTESIAN_POINT ( 'NONE',  ( -10.04281598263999875, 21.50000000000000000, 1.000000000000000000 ) ) ;
#9899 = CARTESIAN_POINT ( 'NONE',  ( 23.41720236907999819, -1.131410883462000028, 9.692640973934999238 ) ) ;
#9900 = B_SPLINE_CURVE_WITH_KNOTS ( 'NONE', 3,
 ( #7140, #23368, #21808, #21403, #19218, #4447, #15817, #15931, #13757, #4817, #10388, #9891, #17281, #11837, #15454, #10261, #2759, #22841 ),
 .UNSPECIFIED., .F., .F.,
 ( 4, 2, 2, 2, 2, 2, 2, 2, 4 ),
 ( 0.000000000000000000, 0.1250000000000000000, 0.2500000000000000000, 0.3750000000000000000, 0.5000000000000000000, 0.6250000000000000000, 0.7500000000000000000, 0.8750000000000000000, 1.000000000000000000 ),
 .UNSPECIFIED. ) ;
#9901 = DIRECTION ( 'NONE',  ( -1.000000000000000000, 0.000000000000000000, 0.000000000000000000 ) ) ;
#9902 = ORIENTED_EDGE ( 'NONE', *, *, #8542, .T. ) ;
#9903 = CARTESIAN_POINT ( 'NONE',  ( 11.61517937764999964, -2.662040662477000108, -8.927692317508000741 ) ) ;
#9904 = CARTESIAN_POINT ( 'NONE',  ( -1.289728978252000058, 28.51913313895000002, -2.104626470933999904 ) ) ;
#9905 = CARTESIAN_POINT ( 'NONE',  ( 4.604941514899001831, 12.48958726761999571, 1.077474224869999775 ) ) ;
#9906 = CARTESIAN_POINT ( 'NONE',  ( 2.159790447331193075, 29.00657262603238351, -0.04485059893192275965 ) ) ;
#9907 = CARTESIAN_POINT ( 'NONE',  ( -24.10776096368000054, 9.886905199420999324, -5.181215075838999873 ) ) ;
#9908 = VERTEX_POINT ( 'NONE', #20557 ) ;
#9909 = CARTESIAN_POINT ( 'NONE',  ( 1.800000000175999926, 13.00000000000000000, 1.081665382745000015 ) ) ;
#9910 = VERTEX_POINT ( 'NONE', #11603 ) ;
#9911 = EDGE_CURVE ( 'NONE', #12880, #9729, #3838, .T. ) ;
#9912 = CARTESIAN_POINT ( 'NONE',  ( 4.749999673578000348, 12.55004296393999930, -4.341645649670000483E-06 ) ) ;
#9913 = CARTESIAN_POINT ( 'NONE',  ( 0.000000000000000000, 26.34999999328000087, 0.000000000000000000 ) ) ;
#9914 = CARTESIAN_POINT ( 'NONE',  ( 3.482092246234998800, 13.23084471460000167, 5.478241207029996396 ) ) ;
#9915 = VECTOR ( 'NONE', #18783, 1000.000000000000000 ) ;
#9916 = CONICAL_SURFACE ( 'NONE', #2569, 9.136555860486998526, 0.02565634000431304615 ) ;
#9917 = DIRECTION ( 'NONE',  ( 1.000000000000000000, 0.000000000000000000, 0.000000000000000000 ) ) ;
#9918 = CARTESIAN_POINT ( 'NONE',  ( 12.12975174931000133, -10.21766741648000121, -2.893652579598999797 ) ) ;
#9919 = CARTESIAN_POINT ( 'NONE',  ( -17.87080258880000017, 5.796842063356000274, 9.195416763971000051 ) ) ;
#9920 = CARTESIAN_POINT ( 'NONE',  ( 16.43793875730999687, -4.200504661774999704, 8.191206307881000015 ) ) ;
#9921 = CARTESIAN_POINT ( 'NONE',  ( 19.05233531832000082, -1.887707665395999879, 10.26617185442000135 ) ) ;
#9922 = VERTEX_POINT ( 'NONE', #7838 ) ;
#9923 = EDGE_CURVE ( 'NONE', #2115, #12128, #7709, .T. ) ;
#9924 = CARTESIAN_POINT ( 'NONE',  ( 2.222509048435000079, 30.93848831202999961, -1.574711173318000146 ) ) ;
#9925 = AXIS2_PLACEMENT_3D ( 'NONE', #9026, #16893, #783 ) ;
#9926 = CARTESIAN_POINT ( 'NONE',  ( 2.474460460966999786, 23.85396990879999990, 0.5055298778630998857 ) ) ;
#9927 = CARTESIAN_POINT ( 'NONE',  ( 13.77916999064124504, -7.232023062304977046, 7.346102567300633268 ) ) ;
#9928 = CIRCLE ( 'NONE', #19211, 3.000000000000000000 ) ;
#9929 = CARTESIAN_POINT ( 'NONE',  ( -0.7454422758268997029, 13.21307987702999576, -6.061668110315994618 ) ) ;
#9930 = CARTESIAN_POINT ( 'NONE',  ( -0.4253681007931999769, 28.35394054784999796, 2.615173885854999991 ) ) ;
#9931 = CARTESIAN_POINT ( 'NONE',  ( 14.58760727575919880, -8.335758281611482801, 3.616921650321700987 ) ) ;
#9932 = CARTESIAN_POINT ( 'NONE',  ( 17.45863886587524760, -10.56286734491478008, -0.7285313845211358608 ) ) ;
#9933 = CARTESIAN_POINT ( 'NONE',  ( 13.50000000000000000, 0.000000000000000000, 0.000000000000000000 ) ) ;
#9934 = DIRECTION ( 'NONE',  ( -1.000000000000000000, 0.000000000000000000, 0.000000000000000000 ) ) ;
#9935 = LINE ( 'NONE', #11644, #13110 ) ;
#9936 = VERTEX_POINT ( 'NONE', #14971 ) ;
#9937 = CARTESIAN_POINT ( 'NONE',  ( -2.402048786002945135, 11.81788909627579187, -4.144620335373454978 ) ) ;
#9938 = ORIENTED_EDGE ( 'NONE', *, *, #14435, .F. ) ;
#9939 = ADVANCED_FACE ( 'NONE', ( #11364 ), #11717, .T. ) ;
#9940 = DIRECTION ( 'NONE',  ( 1.000000000000000000, -0.000000000000000000, -0.000000000000000000 ) ) ;
#9942 = CARTESIAN_POINT ( 'NONE',  ( -2.143277222256999792, 23.64327722226000006, 4.118360636503000477E-13 ) ) ;
#9941 = CARTESIAN_POINT ( 'NONE',  ( -3.805495096816462031, 12.08739645174783739, 2.982851083477900289 ) ) ;
#9943 = CARTESIAN_POINT ( 'NONE',  ( 2.390253620507223786, 12.99717099578450430, 6.277524352174514988 ) ) ;
#9944 = CARTESIAN_POINT ( 'NONE',  ( 16.21568206723000216, -6.556442847978000366, -8.910386729497998815 ) ) ;
#9945 = CARTESIAN_POINT ( 'NONE',  ( -6.166365645201998369, 15.19835549494000304, -2.169414073428999057 ) ) ;
#9946 = CARTESIAN_POINT ( 'NONE',  ( -1.767805011140364924, 26.50018596745192312, 1.767686163102024643 ) ) ;
#9947 = ORIENTED_EDGE ( 'NONE', *, *, #16757, .T. ) ;
#9948 = AXIS2_PLACEMENT_3D ( 'NONE', #9889, #919, #6011 ) ;
#9949 = ORIENTED_EDGE ( 'NONE', *, *, #15286, .F. ) ;
#9950 = CARTESIAN_POINT ( 'NONE',  ( -14.00000000000000000, 3.648514493304280126, -8.539308174521250905 ) ) ;
#9951 = CARTESIAN_POINT ( 'NONE',  ( 3.643546194520566051, 29.79977277844448125, -2.515199777306227347 ) ) ;
#9952 = CARTESIAN_POINT ( 'NONE',  ( -24.11803009771612949, -8.641091274406146994, -10.03259869780779567 ) ) ;
#9953 = CIRCLE ( 'NONE', #10747, 4.649999999999999467 ) ;
#9954 = EDGE_LOOP ( 'NONE', ( #5063, #8430, #11255, #15033, #22629, #5678 ) ) ;
#9955 = ADVANCED_FACE ( 'NONE', ( #21034 ), #21567, .F. ) ;
#9956 = CARTESIAN_POINT ( 'NONE',  ( -18.91721189367000022, -3.796518214708000105, 8.814796721447999417 ) ) ;
#9957 = LINE ( 'NONE', #23023, #5153 ) ;
#9958 = CARTESIAN_POINT ( 'NONE',  ( 4.750000000000000000, 24.29999999999999716, 0.000000000000000000 ) ) ;
#9959 = CARTESIAN_POINT ( 'NONE',  ( 15.77318932640266880, -10.19605645657118487, 1.803564215919225333 ) ) ;
#9960 = CARTESIAN_POINT ( 'NONE',  ( -14.55077782637000006, -1.548327575011000157, 10.89675555037999999 ) ) ;
#9961 = CARTESIAN_POINT ( 'NONE',  ( 2.256627625724999753, 29.58481375689000004, 0.6777845771746999759 ) ) ;
#9962 = CARTESIAN_POINT ( 'NONE',  ( -21.35931016950181416, -10.06206865553333607, 3.097961417847729049 ) ) ;
#9963 = VECTOR ( 'NONE', #23101, 1000.000000000000114 ) ;
#9964 = CARTESIAN_POINT ( 'NONE',  ( 0.000000000000000000, 18.50000000000000000, 0.000000000000000000 ) ) ;
#9965 = EDGE_CURVE ( 'NONE', #5281, #5299, #20870, .T. ) ;
#9966 = CARTESIAN_POINT ( 'NONE',  ( -2.070194703216106991, 29.44071876932419585, 0.6155423327383686694 ) ) ;
#9967 = VERTEX_POINT ( 'NONE', #14603 ) ;
#9968 = CARTESIAN_POINT ( 'NONE',  ( -1.864937606498999978, 24.33875932984999935, -1.428034483940999966 ) ) ;
#9969 = CARTESIAN_POINT ( 'NONE',  ( -16.66239188288299644, 10.06542107247047113, 2.687320209561217865 ) ) ;
#9970 = B_SPLINE_CURVE_WITH_KNOTS ( 'NONE', 3,
 ( #13580, #4504, #15265, #11538, #13222, #13336, #9950, #20734, #7779, #4025, #17337, #18792, #859, #2441, #2203, #8016, #4385, #8144, #15510, #17215, #13457, #9594, #8262, #10079, #612, #15388, #2325, #20974, #22657, #11776, #19278, #2560, #740, #17465, #9716, #19149, #22898, #16979, #6313, #382, #11896, #15626, #17097, #495, #5838, #6066, #15146, #4634, #8746, #10684, #12140, #3065, #23138 ),
 .UNSPECIFIED., .F., .F.,
 ( 4, 1, 1, 1, 1, 1, 2, 2, 1, 1, 1, 1, 1, 1, 2, 2, 1, 1, 1, 2, 2, 1, 1, 1, 2, 2, 1, 1, 1, 1, 2, 2, 1, 1, 1, 1, 2, 2, 4 ),
 ( 0.000000000000000000, 0.1249999999999986122, 0.1874999999999979738, 0.2187499999999976130, 0.2343749999999975020, 0.2421874999999974187, 0.2460937499999973910, 0.2499999999999973355, 0.3124999999999965583, 0.3437499999999961697, 0.3593749999999960032, 0.3671874999999958922, 0.3710937499999958367, 0.3730468749999957812, 0.3740234374999958367, 0.3749999999999958922, 0.4374999999999960587, 0.4687499999999961697, 0.4843749999999962252, 0.4921874999999962808, 0.4999999999999963363, 0.5624999999999965583, 0.5937499999999966693, 0.6093749999999966693, 0.6171874999999966693, 0.6249999999999966693, 0.6874999999999970024, 0.7187499999999972244, 0.7343749999999973355, 0.7421874999999973355, 0.7460937499999973355, 0.7499999999999974465, 0.8124999999999984457, 0.8437499999999988898, 0.8593749999999991118, 0.8671874999999992228, 0.8710937499999993339, 0.8749999999999993339, 1.000000000000000000 ),
 .UNSPECIFIED. ) ;
#9971 = VERTEX_POINT ( 'NONE', #1546 ) ;
#9972 = EDGE_CURVE ( 'NONE', #2993, #18414, #16235, .T. ) ;
#9973 = CARTESIAN_POINT ( 'NONE',  ( 4.720439035602998601, 14.52233946640999562, -3.835351803237996737 ) ) ;
#9974 = CARTESIAN_POINT ( 'NONE',  ( 2.000000000000000000, 28.00000000000000000, -3.464101615137999968 ) ) ;
#9975 = CARTESIAN_POINT ( 'NONE',  ( 12.51562642131000125, 9.466654096131000173, 1.662047859332999922 ) ) ;
#9976 = ORIENTED_EDGE ( 'NONE', *, *, #15472, .F. ) ;
#9977 = CARTESIAN_POINT ( 'NONE',  ( 0.000000000000000000, -1.100000000000000089, 0.000000000000000000 ) ) ;
#9978 = AXIS2_PLACEMENT_3D ( 'NONE', #11619, #13416, #453 ) ;
#9979 = CARTESIAN_POINT ( 'NONE',  ( -0.3272492347489393549, 27.01666666666667282, -2.499999999999999556 ) ) ;
#9980 = CARTESIAN_POINT ( 'NONE',  ( 8.196152422706999729, 26.90192378864669820, -6.000000000000000000 ) ) ;
#9981 = B_SPLINE_SURFACE_WITH_KNOTS ( 'NONE', 3, 3, ( 
 ( #17411, #10026, #17650, #681, #2630, #1179, #804, #23326, #6739, #11963, #23208, #19469, #6253, #8088, #17779, #8205, #15571, #19592, #13887, #22960, #8572, #6376, #14133, #21160, #922, #6505, #4571, #21290, #19352, #6624, #8449, #14013, #21527, #13637, #4941 ),
 ( #12204, #21033, #10141, #17529, #19090, #8323, #12087, #2503, #15688, #23078, #4702, #2879, #3003, #23447, #17898, #7097, #1299, #20183, #6862, #14374, #21767, #1545, #14255, #8690, #21653, #12682, #23580, #7211, #5180, #14716, #9158, #23690, #3369, #5066, #14488 ),
 ( #12448, #6985, #12562, #12794, #14602, #23924, #19948, #3483, #19832, #8930, #10630, #1652, #3245, #8817, #18018, #21998, #16178, #20069, #16054, #1419, #16299, #10746, #21880, #18140, #5289, #10865, #18249, #9041, #16412, #7335, #3592, #5411, #23803, #10976, #18359 ),
 ( #1770, #16535, #22111, #12327, #19718, #3130, #10515, #4061, #3701, #13017, #11574, #11222, #9748, #17134, #22338, #2235, #5872, #16656, #18478, #20771, #14825, #5633, #5986, #292, #2007, #18951, #20417, #2357, #9391, #11340, #16885, #3826, #7694, #172, #9629 ) ),
 .UNSPECIFIED., .F., .F., .F.,
 ( 4, 4 ),
 ( 4, 1, 1, 1, 1, 1, 1, 1, 1, 1, 1, 1, 1, 1, 1, 1, 1, 1, 1, 1, 1, 1, 1, 1, 1, 1, 1, 1, 1, 1, 1, 1, 4 ),
 ( -0.08408083179837000376, 1.084080831798000188 ),
 ( 0.1936290155325000040, 0.2193222086650999936, 0.2450154017976000076, 0.2707085949301000216, 0.2964017880627000112, 0.3220949811952000252, 0.3477881743278000148, 0.3734813674603000289, 0.3991745605929000185, 0.4248677537254000325, 0.4505609468578999910, 0.4762541399905000361, 0.5019473331230001056, 0.5276405262555999842, 0.5533337193880999427, 0.5790269125207000434, 0.6047201056532000019, 0.6304132987856999604, 0.6561064919182999500, 0.6817996850508000195, 0.7074928781834000091, 0.7331860713158999676, 0.7588792644484000371, 0.7845724575810000267, 0.8102656507134999853, 0.8359588438460999749, 0.8616520369785999334, 0.8873452301112000340, 0.9130384232436999925, 0.9387316163761999510, 0.9644248095088000516, 0.9901180026413000101, 1.015811195773999920 ),
 .UNSPECIFIED. ) ;
#9982 = ORIENTED_EDGE ( 'NONE', *, *, #5282, .T. ) ;
#9983 = EDGE_CURVE ( 'NONE', #9190, #8278, #15058, .T. ) ;
#9985 = B_SPLINE_CURVE_WITH_KNOTS ( 'NONE', 3,
 ( #5367, #12757, #5141, #20147, #3554, #5481, #18436, #8644, #12411, #12523 ),
 .UNSPECIFIED., .F., .F.,
 ( 4, 2, 2, 2, 4 ),
 ( 0.000000000000000000, 0.2115962377624443225, 0.4231924755248886449, 0.6347887132873327731, 0.8463849510497769568 ),
 .UNSPECIFIED. ) ;
#9984 = LINE ( 'NONE', #4296, #13478 ) ;
#9986 = CARTESIAN_POINT ( 'NONE',  ( 12.12543434881680149, 8.197779943787733004, 10.80110243426253014 ) ) ;
#9987 = CARTESIAN_POINT ( 'NONE',  ( 24.44127686332184268, -6.767441607451973873, 8.200622886799944666 ) ) ;
#9988 = FACE_OUTER_BOUND ( 'NONE', #13767, .T. ) ;
#9989 = CARTESIAN_POINT ( 'NONE',  ( 17.95021154713298372, -4.863476692990534644, -9.270487928442411985 ) ) ;
#9990 = CONICAL_SURFACE ( 'NONE', #23531, 4.649999926447000220, 0.7853981633972997312 ) ;
#9991 = DIRECTION ( 'NONE',  ( 1.000000000000000000, 0.000000000000000000, 0.000000000000000000 ) ) ;
#9992 = CARTESIAN_POINT ( 'NONE',  ( 11.01624327026000039, 1.089736728551999927E-14, 0.000000000000000000 ) ) ;
#9993 = CARTESIAN_POINT ( 'NONE',  ( 19.90431259713000145, 9.967540672853999695, -5.083098181931998916 ) ) ;
#9994 = CARTESIAN_POINT ( 'NONE',  ( 0.000000000000000000, 26.20000000000000284, 4.618802153517000519 ) ) ;
#9995 = AXIS2_PLACEMENT_3D ( 'NONE', #23230, #950, #19374 ) ;
#9996 = CARTESIAN_POINT ( 'NONE',  ( -2.184465970885646424, 28.96753006952333465, -1.259047450927245126 ) ) ;
#9997 = DIRECTION ( 'NONE',  ( -0.000000000000000000, 1.000000000000000000, 0.000000000000000000 ) ) ;
#9998 = CARTESIAN_POINT ( 'NONE',  ( -1.086675645002173507, 30.07086948948929006, -1.869048572787896489 ) ) ;
#9999 = ORIENTED_EDGE ( 'NONE', *, *, #3445, .T. ) ;
#10000 = CARTESIAN_POINT ( 'NONE',  ( 23.02223177661903364, 8.095646187396759785, 4.666105312640251412 ) ) ;
#10001 = CARTESIAN_POINT ( 'NONE',  ( 24.33785594068000080, -9.240887486209999224, 5.917068627456000485 ) ) ;
#10002 = CARTESIAN_POINT ( 'NONE',  ( -1.358858436891593247, 12.86586849937732069, -6.542507879071220778 ) ) ;
#10003 = FACE_OUTER_BOUND ( 'NONE', #20289, .T. ) ;
#10004 = CIRCLE ( 'NONE', #1509, 10.59999999999999964 ) ;
#10005 = EDGE_CURVE ( 'NONE', #19819, #9734, #14021, .T. ) ;
#10006 = CARTESIAN_POINT ( 'NONE',  ( -20.85848541575246884, -7.716069547171855447, -7.142552263296302328 ) ) ;
#10007 = DIRECTION ( 'NONE',  ( 0.000000000000000000, 0.000000000000000000, -1.000000000000000000 ) ) ;
#10008 = EDGE_CURVE ( 'NONE', #20574, #6561, #2790, .T. ) ;
#10009 = DIRECTION ( 'NONE',  ( 0.000000000000000000, 1.000000000000000000, 0.000000000000000000 ) ) ;
#10010 = ORIENTED_EDGE ( 'NONE', *, *, #11029, .T. ) ;
#10011 = VECTOR ( 'NONE', #12630, 1000.000000000000000 ) ;
#10012 = CARTESIAN_POINT ( 'NONE',  ( -18.07511824061237604, 6.027222043823452502, 8.713521295921685450 ) ) ;
#10013 = CARTESIAN_POINT ( 'NONE',  ( -2.899999929817000055, 18.99999992981999952, -2.312669444528000281E-07 ) ) ;
#10014 = AXIS2_PLACEMENT_3D ( 'NONE', #13766, #10521, #13894 ) ;
#10015 = AXIS2_PLACEMENT_3D ( 'NONE', #9160, #12901, #3703 ) ;
#10016 = CARTESIAN_POINT ( 'NONE',  ( -1.533591067958279819, 27.72982077893267316, 1.536412323194911833 ) ) ;
#10017 = DIRECTION ( 'NONE',  ( -1.000000000000000000, 0.000000000000000000, 0.000000000000000000 ) ) ;
#10018 = DIRECTION ( 'NONE',  ( 0.000000000000000000, 1.000000000000000000, 0.000000000000000000 ) ) ;
#10019 = ORIENTED_EDGE ( 'NONE', *, *, #4022, .T. ) ;
#10020 = CLOSED_SHELL ( 'NONE', ( #21375, #821, #6885, #12658, #23145, #5970, #3170, #3131, #10316, #13959, #3015, #8080, #17060, #15443, #237, #303, #16333, #19350 ) ) ;
#10021 = EDGE_CURVE ( 'NONE', #23288, #16360, #1551, .T. ) ;
#10022 = CARTESIAN_POINT ( 'NONE',  ( 17.56312270046333524, 7.970618670273120543, -4.594122601136384709 ) ) ;
#10023 = ADVANCED_FACE ( 'NONE', ( #21729 ), #13509, .T. ) ;
#10024 = AXIS2_PLACEMENT_3D ( 'NONE', #5642, #7706, #3956 ) ;
#10025 = CARTESIAN_POINT ( 'NONE',  ( 14.43318924931000069, 4.163528467249999920, -9.835102695514999382 ) ) ;
#10026 = CARTESIAN_POINT ( 'NONE',  ( -24.48716916290999990, -3.591176638987999770, -10.24322100536999969 ) ) ;
#10027 = CARTESIAN_POINT ( 'NONE',  ( -16.37566443781999936, 5.581214954223999491, 9.898954454263000358 ) ) ;
#10028 = CARTESIAN_POINT ( 'NONE',  ( 23.85139158929754188, -9.055547910765916697, -2.371671287066565270 ) ) ;
#10029 = CARTESIAN_POINT ( 'NONE',  ( 17.08937451746000136, 1.841749366007999988, -9.602221512397999703 ) ) ;
#10030 = CARTESIAN_POINT ( 'NONE',  ( -7.034000000000000696, 11.50000000000000000, 0.000000000000000000 ) ) ;
#10031 = CARTESIAN_POINT ( 'NONE',  ( 1.536366799937295413, 26.91753006952333749, 1.999167105995444338 ) ) ;
#10032 = CARTESIAN_POINT ( 'NONE',  ( 22.00080955183999976, -9.690658177826998454, 0.7515038182808999601 ) ) ;
#10033 = AXIS2_PLACEMENT_3D ( 'NONE', #11932, #15542, #22930 ) ;
#10034 = CARTESIAN_POINT ( 'NONE',  ( 0.000000000000000000, 19.00000000000000000, 0.000000000000000000 ) ) ;
#10035 = ORIENTED_EDGE ( 'NONE', *, *, #14323, .T. ) ;
#10036 = CARTESIAN_POINT ( 'NONE',  ( 18.85240113949000218, -1.886779804701000041, 10.26112574610000117 ) ) ;
#10037 = CARTESIAN_POINT ( 'NONE',  ( -1.483218624018999954, 26.47956776952000268, 2.219793368323999871 ) ) ;
#10038 = CIRCLE ( 'NONE', #7328, 2.399999999999999911 ) ;
#10039 = CARTESIAN_POINT ( 'NONE',  ( 3.677613186714003835, 12.08831154218000314, 3.066611987921000981 ) ) ;
#10040 = CARTESIAN_POINT ( 'NONE',  ( 2.145115102489369097, 28.98698980757362875, 0.2846114639472765440 ) ) ;
#10041 = CARTESIAN_POINT ( 'NONE',  ( -23.96113936679000034, 9.883381352389999819, -5.179368058338999603 ) ) ;
#10042 = CARTESIAN_POINT ( 'NONE',  ( -14.25000000000000000, 0.000000000000000000, 0.000000000000000000 ) ) ;
#10043 = VECTOR ( 'NONE', #22675, 999.9999999999998863 ) ;
#10044 = ORIENTED_EDGE ( 'NONE', *, *, #13758, .T. ) ;
#10045 = CARTESIAN_POINT ( 'NONE',  ( 0.5097591796037457268, 26.26046041277498233, 2.099534046982708180 ) ) ;
#10046 = CARTESIAN_POINT ( 'NONE',  ( -8.250000000000000000, 22.00000000000000000, 2.500000000000000000 ) ) ;
#10047 = CARTESIAN_POINT ( 'NONE',  ( -0.4498711834209865867, 6.792576835581316530, 1.691454280765045448 ) ) ;
#10048 = DIRECTION ( 'NONE',  ( 0.000000000000000000, 0.9420570860200443430, 0.3354525997505800605 ) ) ;
#10049 = AXIS2_PLACEMENT_3D ( 'NONE', #133, #14788, #18784 ) ;
#10050 = CARTESIAN_POINT ( 'NONE',  ( -19.13034275784999849, -9.231395905450000328, -6.758791263612999423 ) ) ;
#10051 = AXIS2_PLACEMENT_3D ( 'NONE', #6923, #21709, #1356 ) ;
#10052 = CARTESIAN_POINT ( 'NONE',  ( 17.31543875730999815, 3.351454173900000111, -8.598433847594998625 ) ) ;
#10053 = DIRECTION ( 'NONE',  ( -1.000000000000000000, 0.000000000000000000, 0.000000000000000000 ) ) ;
#10054 = ORIENTED_EDGE ( 'NONE', *, *, #20745, .T. ) ;
#10055 = CARTESIAN_POINT ( 'NONE',  ( 19.08782216824772959, -8.814560846539785999, 5.694643456270070736 ) ) ;
#10056 = CARTESIAN_POINT ( 'NONE',  ( -4.000000000000000888, 29.89685207198628092, 1.322601766568780146 ) ) ;
#10057 = CARTESIAN_POINT ( 'NONE',  ( -2.465106068310999987, 25.02935756624999541, 1.140263770482999872 ) ) ;
#10058 = CARTESIAN_POINT ( 'NONE',  ( 4.284596121176959649, 14.56923866457215588, -4.377423833532463782 ) ) ;
#10059 = CARTESIAN_POINT ( 'NONE',  ( -10.04701370327999932, 16.31160201366999729, -1.000000000000000000 ) ) ;
#10060 = CARTESIAN_POINT ( 'NONE',  ( -12.06624327026013077, 13.93375672974000068, 0.000000000000000000 ) ) ;
#10061 = DIRECTION ( 'NONE',  ( 0.000000000000000000, 1.000000000000000000, 0.000000000000000000 ) ) ;
#10062 = CARTESIAN_POINT ( 'NONE',  ( 11.53663804754310718, -3.465671449079424704, 12.49990775414663702 ) ) ;
#10063 = CARTESIAN_POINT ( 'NONE',  ( 17.12411249101483079, -4.802526802559668795, 9.264146113958686257 ) ) ;
#10064 = DIRECTION ( 'NONE',  ( -0.000000000000000000, 1.000000000000000000, 0.000000000000000000 ) ) ;
#10065 = PLANE ( 'NONE',  #11970 ) ;
#10066 = CARTESIAN_POINT ( 'NONE',  ( 1.536366799937286087, 29.55086340285667035, -1.999167105995451221 ) ) ;
#10067 = ORIENTED_EDGE ( 'NONE', *, *, #20310, .T. ) ;
#10068 = FACE_OUTER_BOUND ( 'NONE', #5335, .T. ) ;
#10069 = CARTESIAN_POINT ( 'NONE',  ( 11.85409292833336892, -8.571431512456976876, 10.15389364928055471 ) ) ;
#10070 = ORIENTED_EDGE ( 'NONE', *, *, #314, .F. ) ;
#10071 = CARTESIAN_POINT ( 'NONE',  ( 0.000000000000000000, 18.10000000000000142, 0.000000000000000000 ) ) ;
#10072 = CARTESIAN_POINT ( 'NONE',  ( 1.999167105995460769, 28.55086340285666324, 1.536366799937272765 ) ) ;
#10073 = CARTESIAN_POINT ( 'NONE',  ( -23.74465998031000069, -7.716878364870000340, -11.63397459621999985 ) ) ;
#10074 = CARTESIAN_POINT ( 'NONE',  ( -2.500000000000000000, 18.50000000000000000, 0.000000000000000000 ) ) ;
#10075 = CARTESIAN_POINT ( 'NONE',  ( -20.25016455292000117, -8.657612072530000091, 3.085311466348000131 ) ) ;
#10076 = CARTESIAN_POINT ( 'NONE',  ( 2.322750540216000026, 26.09419433610000283, 1.687576972922000040 ) ) ;
#10077 = ORIENTED_EDGE ( 'NONE', *, *, #9712, .T. ) ;
#10078 = ORIENTED_EDGE ( 'NONE', *, *, #7137, .F. ) ;
#10079 = CARTESIAN_POINT ( 'NONE',  ( -13.99999999999999645, -1.581653827019005920, -9.457174266960452158 ) ) ;
#10080 = CARTESIAN_POINT ( 'NONE',  ( 0.000000000000000000, 20.00000000000000000, 0.000000000000000000 ) ) ;
#10081 = DIRECTION ( 'NONE',  ( 1.000000000000000000, 0.000000000000000000, 0.000000000000000000 ) ) ;
#10082 = ORIENTED_EDGE ( 'NONE', *, *, #21523, .T. ) ;
#10083 = CARTESIAN_POINT ( 'NONE',  ( 0.000000000000000000, 28.00000000000000000, 0.000000000000000000 ) ) ;
#10084 = CARTESIAN_POINT ( 'NONE',  ( 0.000000000000000000, 19.04999994433000055, 0.000000000000000000 ) ) ;
#10085 = CARTESIAN_POINT ( 'NONE',  ( 14.88759896974780972, 10.27467121929758420, -1.078508883751306380 ) ) ;
#10086 = CARTESIAN_POINT ( 'NONE',  ( -15.84946274974000069, -10.91352918511999981, 1.678437607090999872 ) ) ;
#10087 = EDGE_CURVE ( 'NONE', #18064, #22068, #9985, .T. ) ;
#10088 = CARTESIAN_POINT ( 'NONE',  ( -1.933408640761000052, 29.94449886025999774, -1.346733530429999881 ) ) ;
#10089 = CARTESIAN_POINT ( 'NONE',  ( -21.28210479225873542, -10.51966893827426297, 0.3278972208331196181 ) ) ;
#10090 = CARTESIAN_POINT ( 'NONE',  ( -13.44269301469999967, -0.9911996677733001526, -11.23901760903999936 ) ) ;
#10091 = CARTESIAN_POINT ( 'NONE',  ( -0.5972122245493562964, 29.56816721632387512, 2.075699671229644050 ) ) ;
#10092 = ORIENTED_EDGE ( 'NONE', *, *, #17257, .F. ) ;
#10093 = CARTESIAN_POINT ( 'NONE',  ( 2.116385362157999772, 23.95644821291999804, 0.5468322576709999661 ) ) ;
#10094 = CARTESIAN_POINT ( 'NONE',  ( -15.50482492894748177, -4.417095855546814498, -9.394177675399193461 ) ) ;
#10095 = ORIENTED_EDGE ( 'NONE', *, *, #973, .T. ) ;
#10096 = CARTESIAN_POINT ( 'NONE',  ( -1.016515298417790758, 24.56303148589417518, -2.109700942474796115 ) ) ;
#10097 = CARTESIAN_POINT ( 'NONE',  ( 6.588726970868003185, 13.51086646594001195, -0.8681320947235999785 ) ) ;
#10098 = EDGE_CURVE ( 'NONE', #13096, #12723, #20490, .T. ) ;
#10099 = CARTESIAN_POINT ( 'NONE',  ( -4.790823927418967898, 13.32134166212725113, -5.557028280688768973 ) ) ;
#10100 = CARTESIAN_POINT ( 'NONE',  ( 1.699986957659999964, 9.000014576061998284, -0.8485216275457999613 ) ) ;
#10101 = CARTESIAN_POINT ( 'NONE',  ( 12.07687642131000061, 2.140746470509000243, -9.358182000212998730 ) ) ;
#10102 = VERTEX_POINT ( 'NONE', #22422 ) ;
#10103 = CARTESIAN_POINT ( 'NONE',  ( -5.833999999999999631, -11.50000000000000000, 0.000000000000000000 ) ) ;
#10104 = CARTESIAN_POINT ( 'NONE',  ( -1.536366799937290084, 27.08333333333333570, -1.999167105995448113 ) ) ;
#10105 = FACE_OUTER_BOUND ( 'NONE', #7316, .T. ) ;
#10106 = EDGE_LOOP ( 'NONE', ( #918, #9202, #445, #17837, #9491 ) ) ;
#10107 = DIRECTION ( 'NONE',  ( 0.000000000000000000, 1.000000000000000000, 0.000000000000000000 ) ) ;
#10108 = CARTESIAN_POINT ( 'NONE',  ( -10.90000000000000036, 7.100000000000000533, 1.377912020595000118E-10 ) ) ;
#10109 = CARTESIAN_POINT ( 'NONE',  ( 24.17654558719286229, 2.389057866675304176, 10.34701704806261446 ) ) ;
#10110 = CARTESIAN_POINT ( 'NONE',  ( 4.000000000000000000, 26.29977277844473349, 1.897803675662218970 ) ) ;
#10111 = CARTESIAN_POINT ( 'NONE',  ( 18.05946651195386110, -1.087382630457392141, -10.35418620074316287 ) ) ;
#10112 = CARTESIAN_POINT ( 'NONE',  ( 0.000000000000000000, 31.00000000000000000, 0.000000000000000000 ) ) ;
#10113 = EDGE_CURVE ( 'NONE', #4168, #16663, #18928, .T. ) ;
#10114 = CARTESIAN_POINT ( 'NONE',  ( -14.49284524109529038, -11.34356441105103919, 5.352320976844065825 ) ) ;
#10115 = CARTESIAN_POINT ( 'NONE',  ( 24.45606130522000399, -6.841511667768999772, 9.010092832684000186 ) ) ;
#10116 = CARTESIAN_POINT ( 'NONE',  ( 2.267779804951839839, 26.36777980495183726, 5.387954023152814032E-08 ) ) ;
#10117 = CARTESIAN_POINT ( 'NONE',  ( -3.666321194958030105, 14.29055989747922339, -4.906588955330460244 ) ) ;
#10118 = CARTESIAN_POINT ( 'NONE',  ( 23.41677564524290744, 37.01856778792605240, 6.000000000000000000 ) ) ;
#10119 = CARTESIAN_POINT ( 'NONE',  ( -1.595082304731897826, 30.10957549855011450, -1.456253076787439094 ) ) ;
#10120 = ORIENTED_EDGE ( 'NONE', *, *, #13203, .F. ) ;
#10121 = CARTESIAN_POINT ( 'NONE',  ( 23.13555403315795544, 5.650293567432652431, 7.367300352106260775 ) ) ;
#10122 = CARTESIAN_POINT ( 'NONE',  ( 18.68101713701000222, -9.202032660154998212, 4.584888180875999808 ) ) ;
#10123 = CARTESIAN_POINT ( 'NONE',  ( -3.418248095344834869, 13.19611224794727100, -5.848127910700672949 ) ) ;
#10124 = DIRECTION ( 'NONE',  ( -1.209279329285239001E-08, -0.5796072251201023207, -0.8148959839075015088 ) ) ;
#10125 = CARTESIAN_POINT ( 'NONE',  ( -20.29618154032203492, 9.469680736381290487, -4.539250907894071929 ) ) ;
#10126 = CARTESIAN_POINT ( 'NONE',  ( -14.00000000000000000, 6.995278287856000254, -5.711120943918999160 ) ) ;
#10127 = EDGE_CURVE ( 'NONE', #15019, #3493, #17786, .T. ) ;
#10128 = CARTESIAN_POINT ( 'NONE',  ( 4.940723990893003403, 12.51283213654998505, 0.1566900733660998302 ) ) ;
#10129 = ORIENTED_EDGE ( 'NONE', *, *, #7999, .F. ) ;
#10130 = CARTESIAN_POINT ( 'NONE',  ( -14.05590007961454013, -7.031665520223276289, 7.590363941843731865 ) ) ;
#10131 = AXIS2_PLACEMENT_3D ( 'NONE', #17986, #16143, #19396 ) ;
#10132 = CARTESIAN_POINT ( 'NONE',  ( -4.000000000000001776, 29.99040384242091761, -0.4670641126940870413 ) ) ;
#10133 = CARTESIAN_POINT ( 'NONE',  ( -1.094146582940317858, 27.49559246110014854, -1.910274834462101223 ) ) ;
#10134 = APPLICATION_PROTOCOL_DEFINITION ( 'draft international standard', 'automotive_design', 1998, #6482 ) ;
#10135 = ORIENTED_EDGE ( 'NONE', *, *, #13260, .F. ) ;
#10136 = ORIENTED_EDGE ( 'NONE', *, *, #10145, .F. ) ;
#10137 = CARTESIAN_POINT ( 'NONE',  ( 12.52688711657000020, 13.93375672974000068, -0.8660254037843999608 ) ) ;
#10138 = CIRCLE ( 'NONE', #23677, 16.43375672870000415 ) ;
#10139 = CARTESIAN_POINT ( 'NONE',  ( 16.95600174931000126, 3.031816831187000183, 10.30986099653000032 ) ) ;
#10140 = B_SPLINE_CURVE_WITH_KNOTS ( 'NONE', 3,
 ( #6883, #3023, #18165, #1321, #14279, #23346, #21673, #6765, #18037, #5312, #1443, #16319, #17803, #14156, #1566, #1198, #16202, #23602 ),
 .UNSPECIFIED., .F., .F.,
 ( 4, 2, 2, 2, 2, 2, 2, 2, 4 ),
 ( 0.000000000000000000, 0.1250000000000000000, 0.2500000000000000000, 0.3750000000000000000, 0.5000000000000000000, 0.6250000000000000000, 0.7500000000000000000, 0.8750000000000000000, 1.000000000000000000 ),
 .UNSPECIFIED. ) ;
#10141 = CARTESIAN_POINT ( 'NONE',  ( -24.64929215829999976, 0.3828329976861000183, -10.71529421017999972 ) ) ;
#10142 = EDGE_CURVE ( 'NONE', #20600, #6219, #3474, .T. ) ;
#10143 = CARTESIAN_POINT ( 'NONE',  ( -15.22293278740000133, 10.31197045934999856, -3.197427357995000108 ) ) ;
#10144 = CARTESIAN_POINT ( 'NONE',  ( 22.56966666666665944, 4.658591883815835999, -8.082977972024316671 ) ) ;
#10145 = EDGE_CURVE ( 'NONE', #12220, #13163, #16845, .T. ) ;
#10146 = CARTESIAN_POINT ( 'NONE',  ( 16.68312451746000136, -9.163211135683999586, -3.377722033148000236 ) ) ;
#10147 = DIRECTION ( 'NONE',  ( 0.000000000000000000, 0.000000000000000000, -1.000000000000000000 ) ) ;
#10148 = B_SPLINE_CURVE_WITH_KNOTS ( 'NONE', 3,
 ( #12436, #14362, #16286, #6847, #7086, #14476, #20053, #21868, #5277, #21983, #17886, #21637 ),
 .UNSPECIFIED., .F., .F.,
 ( 4, 1, 1, 1, 1, 2, 2, 4 ),
 ( 0.000000000000000000, 0.2500000000000041633, 0.3750000000000059952, 0.4375000000000063838, 0.4687500000000064948, 0.4843750000000064393, 0.5000000000000064393, 1.000000000000000000 ),
 .UNSPECIFIED. ) ;
#10149 = DIRECTION ( 'NONE',  ( -1.000000000000000000, 0.000000000000000000, 0.000000000000000000 ) ) ;
#10150 = CARTESIAN_POINT ( 'NONE',  ( 24.36881528991178669, -9.280258940103371046, 8.926120008345273860 ) ) ;
#10151 = EDGE_LOOP ( 'NONE', ( #10696, #11913, #11564, #3037 ) ) ;
#10152 = CARTESIAN_POINT ( 'NONE',  ( 0.1267126835535345164, 13.69169213017725362, 6.123708248830501688 ) ) ;
#10153 = CARTESIAN_POINT ( 'NONE',  ( 0.05636985319968000618, 27.46250240009999999, 2.870524099806999629 ) ) ;
#10154 = AXIS2_PLACEMENT_3D ( 'NONE', #15628, #613, #742 ) ;
#10155 = CARTESIAN_POINT ( 'NONE',  ( -1.048427594716000222, 11.59808701839000200, 4.637028203793000181 ) ) ;
#10156 = CARTESIAN_POINT ( 'NONE',  ( 2.649085689637680652, 26.47444252552741872, 3.089351817498230623 ) ) ;
#10157 = CARTESIAN_POINT ( 'NONE',  ( -24.42146710634000328, 5.447078518068000363, -9.752648862749000003 ) ) ;
#10158 = EDGE_CURVE ( 'NONE', #3791, #12959, #345, .T. ) ;
#10159 = EDGE_CURVE ( 'NONE', #15280, #22896, #9586, .T. ) ;
#10160 = DIRECTION ( 'NONE',  ( 0.000000000000000000, -1.000000000000000000, 0.000000000000000000 ) ) ;
#10161 = EDGE_LOOP ( 'NONE', ( #3782, #6850, #21328, #1530 ) ) ;
#10162 = DIRECTION ( 'NONE',  ( -1.000000000000000000, 0.000000000000000000, 0.000000000000000000 ) ) ;
#10163 =( BOUNDED_SURFACE ( )  B_SPLINE_SURFACE ( 3, 3, ( 
 ( #2223, #9616, #23164, #2583, #10097, #17485, #15892, #17735, #3086, #879, #6584, #17360, #2715, #19674, #13596, #4896, #11918 ),
 ( #10347, #19303, #13718, #20994, #1137, #10472, #12161, #21113, #14087, #15530, #762, #4404, #11795, #13969, #17859, #23283, #8534 ),
 ( #6335, #15409, #4527, #8163, #10217, #8282, #12042, #12284, #19551, #2957, #1255, #22917, #4656, #6696, #19174, #21484, #9973 ),
 ( #21360, #17611, #15646, #23038, #6457, #13842, #22798, #6213, #21242, #19425, #2837, #1004, #8407, #15774, #4776, #5858, #22324 ) ),
 .UNSPECIFIED., .F., .F., .T. ) 
 B_SPLINE_SURFACE_WITH_KNOTS ( ( 4, 4 ),
 ( 4, 1, 1, 1, 1, 1, 1, 1, 1, 1, 1, 1, 1, 1, 4 ),
 ( 0.000000000000000000, 1.000000000000000000 ),
 ( 0.2368937211084000127, 0.2409453982507999970, 0.2486681467527000200, 0.2559696437135000058, 0.2630400535103000204, 0.2700208015615999657, 0.2769718879389000410, 0.2839229647372999987, 0.2909371157855999979, 0.2981017146652999994, 0.3055324712384000496, 0.3134565545379999763, 0.3221580657204000109, 0.3317495705149000051, 0.3322945160429999767 ),
 .UNSPECIFIED. ) 
 GEOMETRIC_REPRESENTATION_ITEM ( )  RATIONAL_B_SPLINE_SURFACE ( (
 ( 1.093546124775000017, 1.093546124775000017, 1.093546124775000017, 1.093546124775000017, 1.093546124775000017, 1.093546124775000017, 1.093546124775000017, 1.093546124775000017, 1.093546124775000017, 1.093546124775000017, 1.093546124775000017, 1.093546124775000017, 1.093546124775000017, 1.093546124775000017, 1.093546124775000017, 1.093546124775000017, 1.093546124775000017),
 ( 0.9688179584082000639, 0.9688179584082000639, 0.9688179584082000639, 0.9688179584082000639, 0.9688179584082000639, 0.9688179584082000639, 0.9688179584082000639, 0.9688179584082000639, 0.9688179584082000639, 0.9688179584082000639, 0.9688179584082000639, 0.9688179584082000639, 0.9688179584082000639, 0.9688179584082000639, 0.9688179584082000639, 0.9688179584082000639, 0.9688179584082000639),
 ( 0.9688179584082000639, 0.9688179584082000639, 0.9688179584082000639, 0.9688179584082000639, 0.9688179584082000639, 0.9688179584082000639, 0.9688179584082000639, 0.9688179584082000639, 0.9688179584082000639, 0.9688179584082000639, 0.9688179584082000639, 0.9688179584082000639, 0.9688179584082000639, 0.9688179584082000639, 0.9688179584082000639, 0.9688179584082000639, 0.9688179584082000639),
 ( 1.093546124775000017, 1.093546124775000017, 1.093546124775000017, 1.093546124775000017, 1.093546124775000017, 1.093546124775000017, 1.093546124775000017, 1.093546124775000017, 1.093546124775000017, 1.093546124775000017, 1.093546124775000017, 1.093546124775000017, 1.093546124775000017, 1.093546124775000017, 1.093546124775000017, 1.093546124775000017, 1.093546124775000017) ) ) 
 REPRESENTATION_ITEM ( '' )  SURFACE ( )  );
#10164 = DIRECTION ( 'NONE',  ( 1.000000000000000000, 0.000000000000000000, 0.000000000000000000 ) ) ;
#10165 = CARTESIAN_POINT ( 'NONE',  ( -3.194868910741000434, 13.69705038741999026, 5.170042636081004339 ) ) ;
#10166 = CARTESIAN_POINT ( 'NONE',  ( -2.000000000000000000, 24.50000000000000000, -3.464101615137999968 ) ) ;
#10167 = FACE_BOUND ( 'NONE', #10859, .T. ) ;
#10168 = CARTESIAN_POINT ( 'NONE',  ( 2.434931691670788823, 27.06753006952333607, -0.6543697108982007293 ) ) ;
#10169 = CARTESIAN_POINT ( 'NONE',  ( -18.92721240987999920, -2.665110294750000275, -11.12003873501999962 ) ) ;
#10170 = CARTESIAN_POINT ( 'NONE',  ( 14.90231375730999908, -9.084442286569000657, 1.213034410125000129 ) ) ;
#10171 = CARTESIAN_POINT ( 'NONE',  ( 0.3272492347489455167, 27.41666666666666075, 2.499999999999998668 ) ) ;
#10172 = ORIENTED_EDGE ( 'NONE', *, *, #8184, .F. ) ;
#10173 = CARTESIAN_POINT ( 'NONE',  ( -22.04021495466848179, -8.997463528116268705, 2.418937047195946821 ) ) ;
#10174 = CARTESIAN_POINT ( 'NONE',  ( -0.3310328303844999875, 30.17125647670999911, -2.511084930423000294 ) ) ;
#10175 = CARTESIAN_POINT ( 'NONE',  ( -12.25000000000000000, 6.489681479813073750, -13.21205004727046095 ) ) ;
#10176 = CARTESIAN_POINT ( 'NONE',  ( 4.120403429707917731, 14.50536380480940046, -4.532139194909468927 ) ) ;
#10177 = ORIENTED_EDGE ( 'NONE', *, *, #18938, .T. ) ;
#10178 = CARTESIAN_POINT ( 'NONE',  ( -4.105070514359999478, 13.44465293295000485, -4.977031060933996720 ) ) ;
#10179 = CARTESIAN_POINT ( 'NONE',  ( 2.590247180112999814, 28.61723979505000059, -0.9106673404492000579 ) ) ;
#10180 = CARTESIAN_POINT ( 'NONE',  ( -2.000000000000000000, 18.72912878474779319, -6.650110356573455395E-11 ) ) ;
#10181 = CARTESIAN_POINT ( 'NONE',  ( 16.34355094967408917, 8.336021693863266080, -6.395580416082841779 ) ) ;
#10182 = CARTESIAN_POINT ( 'NONE',  ( 23.99062354302999722, -6.216878364870000340, -12.50000000000000000 ) ) ;
#10183 = CARTESIAN_POINT ( 'NONE',  ( 8.124934037954998800, -12.44999999999999929, 0.000000000000000000 ) ) ;
#10184 = CARTESIAN_POINT ( 'NONE',  ( 19.90620603379666420, 2.403516248286488910, 8.943079757202132996 ) ) ;
#10185 = EDGE_LOOP ( 'NONE', ( #981, #16670 ) ) ;
#10186 = LINE ( 'NONE', #10307, #3477 ) ;
#10187 = AXIS2_PLACEMENT_3D ( 'NONE', #17773, #5919, #12081 ) ;
#10188 = CARTESIAN_POINT ( 'NONE',  ( 11.22311500625620795, -9.824279701762014483, 7.983827916374445444 ) ) ;
#10189 = EDGE_LOOP ( 'NONE', ( #404, #22020, #8779, #11794 ) ) ;
#10190 = CARTESIAN_POINT ( 'NONE',  ( -1.703175425154000111, 25.54551418205999980, -2.142696604598000043 ) ) ;
#10191 = DIRECTION ( 'NONE',  ( 0.9063077870366026412, 0.000000000000000000, -0.4226182617408008602 ) ) ;
#10192 = CARTESIAN_POINT ( 'NONE',  ( -4.544324455327999779, 13.49053734526000170, 5.132126114358000812 ) ) ;
#10193 = CARTESIAN_POINT ( 'NONE',  ( 6.141065375610000210, 14.19649368052000149, -1.893142280157000292E-06 ) ) ;
#10194 = CARTESIAN_POINT ( 'NONE',  ( 11.01624327026000039, 1.089736728551999927E-14, 0.000000000000000000 ) ) ;
#10195 = CARTESIAN_POINT ( 'NONE',  ( 2.870524099806999629, 26.97169433610000411, 0.05636985319957999591 ) ) ;
#10196 = ORIENTED_EDGE ( 'NONE', *, *, #12666, .F. ) ;
#10197 = CARTESIAN_POINT ( 'NONE',  ( -2.500000000000000444, 29.85086340285667461, 0.3272492347489422415 ) ) ;
#10198 = CARTESIAN_POINT ( 'NONE',  ( 4.000000000000000000, 29.69999999999999929, -2.309401076759000304 ) ) ;
#10199 = DIRECTION ( 'NONE',  ( 0.000000000000000000, -1.000000000000000000, 0.000000000000000000 ) ) ;
#10200 = ORIENTED_EDGE ( 'NONE', *, *, #13389, .F. ) ;
#10201 = CARTESIAN_POINT ( 'NONE',  ( -24.27577904266999909, 0.9982065492062000001, -11.26793000443000103 ) ) ;
#10202 = DIRECTION ( 'NONE',  ( 1.000000000000000000, 0.000000000000000000, 0.000000000000000000 ) ) ;
#10203 = CARTESIAN_POINT ( 'NONE',  ( 2.500000000000000000, 18.50000000000000000, 0.000000000000000000 ) ) ;
#10204 = CARTESIAN_POINT ( 'NONE',  ( 15.13684082370412654, 7.510860090511030762, 7.114097475440270379 ) ) ;
#10205 = CARTESIAN_POINT ( 'NONE',  ( -17.08006423682000019, 7.985046582893999378, -7.675080017633000296 ) ) ;
#10206 = DIRECTION ( 'NONE',  ( 0.000000000000000000, 0.9998843904358519774, 0.01520545174352925036 ) ) ;
#10207 = CARTESIAN_POINT ( 'NONE',  ( -20.14975925936147760, 7.687190990672447377, 7.145965227562199651 ) ) ;
#10208 = CARTESIAN_POINT ( 'NONE',  ( -4.681494469480999676, 12.59157765981999688, -0.7804412716255002547 ) ) ;
#10209 = CARTESIAN_POINT ( 'NONE',  ( -4.750000000000000000, 20.10000000000000142, 0.000000000000000000 ) ) ;
#10210 = AXIS2_PLACEMENT_3D ( 'NONE', #23204, #2997, #4936 ) ;
#10211 = CARTESIAN_POINT ( 'NONE',  ( -2.071762217469759193, 29.44039273301211423, 0.6102428019939168946 ) ) ;
#10212 = ORIENTED_EDGE ( 'NONE', *, *, #19952, .T. ) ;
#10213 = CARTESIAN_POINT ( 'NONE',  ( 1.521291192730000130, 23.88665044741999921, 1.569645106012999891 ) ) ;
#10214 = CARTESIAN_POINT ( 'NONE',  ( -17.53056709833472837, -9.766724693011614278, -4.094736955089503638 ) ) ;
#10215 = ORIENTED_EDGE ( 'NONE', *, *, #9682, .F. ) ;
#10216 = DIRECTION ( 'NONE',  ( -1.000000000000000000, 0.000000000000000000, 0.000000000000000000 ) ) ;
#10217 = CARTESIAN_POINT ( 'NONE',  ( 6.034210908571004062, 14.08836922021000504, -0.7813677579985999211 ) ) ;
#10218 = CARTESIAN_POINT ( 'NONE',  ( 12.00000000000000178, 0.6217777569271694116, -8.958706245662780177 ) ) ;
#10219 = CARTESIAN_POINT ( 'NONE',  ( 0.000000000000000000, 17.00000000000000000, -3.099999999999986766 ) ) ;
#10220 = VECTOR ( 'NONE', #4020, 1000.000000000000000 ) ;
#10221 = ADVANCED_FACE ( 'NONE', ( #18561 ), #6552, .F. ) ;
#10222 = CARTESIAN_POINT ( 'NONE',  ( 15.25781392131000125, -9.389200645904999476, -2.369324833533999808 ) ) ;
#10223 = EDGE_LOOP ( 'NONE', ( #10687, #20533, #17187, #3811 ) ) ;
#10224 = CARTESIAN_POINT ( 'NONE',  ( 1.414030196417156471E-05, 28.49937488120688656, 2.386519462589231200 ) ) ;
#10225 = DIRECTION ( 'NONE',  ( -1.000000000000000000, 0.000000000000000000, 0.000000000000000000 ) ) ;
#10226 = DIRECTION ( 'NONE',  ( -1.000000000000000000, 0.000000000000000000, 0.000000000000000000 ) ) ;
#10227 = ORIENTED_EDGE ( 'NONE', *, *, #22137, .T. ) ;
#10228 = DIRECTION ( 'NONE',  ( -1.000000000000000000, 0.000000000000000000, 0.000000000000000000 ) ) ;
#10229 = CYLINDRICAL_SURFACE ( 'NONE', #8196, 7.000000000000000000 ) ;
#10230 = CARTESIAN_POINT ( 'NONE',  ( -23.28041318627592560, 8.640587636776928093, -3.475811032938793232 ) ) ;
#10231 = CARTESIAN_POINT ( 'NONE',  ( -14.00000000000000178, 0.4357667221639321409, 9.714757508063044611 ) ) ;
#10232 = CARTESIAN_POINT ( 'NONE',  ( 16.27407322926296018, -0.09559760970984292061, -10.36543711007276869 ) ) ;
#10233 = CARTESIAN_POINT ( 'NONE',  ( 11.99999999999999822, -8.403351023270348108, -5.300159557665803156 ) ) ;
#10234 = EDGE_CURVE ( 'NONE', #7505, #7147, #4261, .T. ) ;
#10235 = CARTESIAN_POINT ( 'NONE',  ( -14.45529013989012412, 12.11766535962173208, -4.011530336787274997 ) ) ;
#10236 = CARTESIAN_POINT ( 'NONE',  ( 21.70285686071999720, 5.756918313552000122, -9.651675814321999169 ) ) ;
#10237 = DIRECTION ( 'NONE',  ( -1.000000000000000000, 0.000000000000000000, 0.000000000000000000 ) ) ;
#10238 = CIRCLE ( 'NONE', #16411, 7.500000000000000000 ) ;
#10239 = CARTESIAN_POINT ( 'NONE',  ( -4.156717377435044547, 13.71198257401902687, -4.893767653246960947 ) ) ;
#10240 = FACE_OUTER_BOUND ( 'NONE', #160, .T. ) ;
#10241 = CARTESIAN_POINT ( 'NONE',  ( -2.159905846019499531, 30.20377729254098753, 0.001675619632035371676 ) ) ;
#10242 = ORIENTED_EDGE ( 'NONE', *, *, #9075, .F. ) ;
#10243 = CARTESIAN_POINT ( 'NONE',  ( 24.53110687423999892, -10.92244599102000002, -1.095095512714000074 ) ) ;
#10244 = CARTESIAN_POINT ( 'NONE',  ( 24.50000000000000000, -2.116736914405999759, 10.36413001332999961 ) ) ;
#10245 = CARTESIAN_POINT ( 'NONE',  ( 0.000000000000000000, 30.00000000000000000, 0.000000000000000000 ) ) ;
#10246 = AXIS2_PLACEMENT_3D ( 'NONE', #11789, #3078, #19292 ) ;
#10247 = CARTESIAN_POINT ( 'NONE',  ( -19.41256116464168358, -9.053821575032303670, 5.280908075822353887 ) ) ;
#10248 = DIRECTION ( 'NONE',  ( 0.000000000000000000, 1.000000000000000000, 0.000000000000000000 ) ) ;
#10249 = CARTESIAN_POINT ( 'NONE',  ( 0.6124999999999999334, 1.217145837503000065E-14, 0.000000000000000000 ) ) ;
#10250 = VERTEX_POINT ( 'NONE', #248 ) ;
#10251 = EDGE_CURVE ( 'NONE', #21017, #20281, #15769, .T. ) ;
#10252 = CARTESIAN_POINT ( 'NONE',  ( -14.00000000000000000, -8.319952449050001420, 6.066771132503999020 ) ) ;
#10253 = DIRECTION ( 'NONE',  ( 1.000000000000000000, 0.000000000000000000, 0.000000000000000000 ) ) ;
#10254 = TOROIDAL_SURFACE ( 'NONE', #7931, 1.600000000000000089, 0.1000000000000000056 ) ;
#10255 = CARTESIAN_POINT ( 'NONE',  ( 2.110282791597058782, 26.46005674015626496, -0.5113919139037653716 ) ) ;
#10256 = CARTESIAN_POINT ( 'NONE',  ( 0.000000000000000000, 0.000000000000000000, 0.000000000000000000 ) ) ;
#10257 = DIRECTION ( 'NONE',  ( 0.000000000000000000, -1.000000000000000000, 0.000000000000000000 ) ) ;
#10258 = ORIENTED_EDGE ( 'NONE', *, *, #195, .F. ) ;
#10259 = FACE_OUTER_BOUND ( 'NONE', #11557, .T. ) ;
#10260 = CARTESIAN_POINT ( 'NONE',  ( -5.240876798540814896, 16.01407665191462826, -3.181876338824043415 ) ) ;
#10261 = CARTESIAN_POINT ( 'NONE',  ( -14.05911075881999217, 5.716256198029335600, -7.053914683086397908 ) ) ;
#10262 = EDGE_CURVE ( 'NONE', #18988, #13308, #23173, .T. ) ;
#10263 = CARTESIAN_POINT ( 'NONE',  ( -17.45736661507000065, -2.009541073283000134, -10.67100981108000113 ) ) ;
#10264 = CARTESIAN_POINT ( 'NONE',  ( -6.299306890445001805, 15.85649737466999376, 1.061595304832000819 ) ) ;
#10265 = CARTESIAN_POINT ( 'NONE',  ( 16.88624951746000136, -4.804895915039999466, -8.508643533405999548 ) ) ;
#10266 = CARTESIAN_POINT ( 'NONE',  ( -0.4920218899694317471, 28.43348844177958767, -2.148916380170569074 ) ) ;
#10267 = DIRECTION ( 'NONE',  ( -0.5000000000000169864, 0.000000000000000000, 0.8660254037844289376 ) ) ;
#10268 = CARTESIAN_POINT ( 'NONE',  ( 0.000000000000000000, 9.000000000000000000, 0.000000000000000000 ) ) ;
#10269 = ORIENTED_EDGE ( 'NONE', *, *, #763, .F. ) ;
#10270 = CARTESIAN_POINT ( 'NONE',  ( -1.349229317769153669, 13.77424421209987493, 5.987165240414223710 ) ) ;
#10271 = CARTESIAN_POINT ( 'NONE',  ( 0.04450989311249999719, 27.14619850837999948, 2.266578917753999889 ) ) ;
#10272 = ADVANCED_FACE ( 'NONE', ( #7406 ), #4643, .F. ) ;
#10273 = CARTESIAN_POINT ( 'NONE',  ( 0.000000000000000000, 28.30000000000000071, 0.000000000000000000 ) ) ;
#10274 = CARTESIAN_POINT ( 'NONE',  ( -14.51889506019236187, 1.113324017026137591, -8.974614630071492627 ) ) ;
#10275 = CARTESIAN_POINT ( 'NONE',  ( -2.437731244915000151, 27.80187716036000367, -0.2400955718763000124 ) ) ;
#10276 = CARTESIAN_POINT ( 'NONE',  ( 0.000000000000000000, 18.89999999999999858, 0.000000000000000000 ) ) ;
#10277 = VERTEX_POINT ( 'NONE', #22297 ) ;
#10278 = CARTESIAN_POINT ( 'NONE',  ( -23.75083293572999921, -13.93375672974000068, 0.6735967263616999823 ) ) ;
#10279 = EDGE_CURVE ( 'NONE', #6884, #19752, #12380, .T. ) ;
#10280 = CARTESIAN_POINT ( 'NONE',  ( 2.490830186055004614, 11.74568911763879164, -4.128140691158040276 ) ) ;
#10281 = CARTESIAN_POINT ( 'NONE',  ( -1.552755157686999787, 13.31391601496999932, 5.888554406491995685 ) ) ;
#10282 = EDGE_CURVE ( 'NONE', #12159, #5281, #21254, .T. ) ;
#10283 = CARTESIAN_POINT ( 'NONE',  ( -0.3690988594039858461, 6.787862677517462195, 1.710243926673669979 ) ) ;
#10284 = DIRECTION ( 'NONE',  ( 0.000000000000000000, -1.000000000000000000, 0.000000000000000000 ) ) ;
#10285 = VECTOR ( 'NONE', #5847, 1000.000000000000000 ) ;
#10286 = CARTESIAN_POINT ( 'NONE',  ( -9.276082211694999913, 14.45305202397999977, -4.386103535306999923 ) ) ;
#10287 = CARTESIAN_POINT ( 'NONE',  ( -15.88025719033000094, -8.846829628555999747, 7.110504558004000053 ) ) ;
#10288 = VECTOR ( 'NONE', #15773, 1000.000000000000000 ) ;
#10289 = CARTESIAN_POINT ( 'NONE',  ( 14.16093892131000054, 8.852644193975999443, -3.852777470446999697 ) ) ;
#10290 = CARTESIAN_POINT ( 'NONE',  ( 18.93357673398348950, 2.325285191727461065, 10.17219493548470943 ) ) ;
#10291 = EDGE_LOOP ( 'NONE', ( #8313, #19700, #6040, #20588, #22857, #13518, #18334, #23817, #4568, #11819, #17427 ) ) ;
#10292 = ADVANCED_FACE ( 'NONE', ( #9704 ), #15255, .T. ) ;
#10293 = DIRECTION ( 'NONE',  ( -1.000000000000000000, 0.000000000000000000, 0.000000000000000000 ) ) ;
#10294 = CARTESIAN_POINT ( 'NONE',  ( 1.910771868463999823, 30.72761905088000134, -1.353836472813999992 ) ) ;
#10295 = CARTESIAN_POINT ( 'NONE',  ( 30.87226923053214378, 35.51856778792605240, 2.673746900119611247 ) ) ;
#10296 = CARTESIAN_POINT ( 'NONE',  ( 2.083048159898164275, 13.90352997106202260, -5.759917838137451618 ) ) ;
#10297 = VERTEX_POINT ( 'NONE', #1847 ) ;
#10298 = DIRECTION ( 'NONE',  ( 0.000000000000000000, -1.000000000000000000, 0.000000000000000000 ) ) ;
#10299 = CARTESIAN_POINT ( 'NONE',  ( 0.000000000000000000, 24.65000000000000213, -4.309401076758999416 ) ) ;
#10300 = DIRECTION ( 'NONE',  ( 0.000000000000000000, -1.000000000000000000, 0.000000000000000000 ) ) ;
#10301 = DIRECTION ( 'NONE',  ( 1.000000000000000000, 0.000000000000000000, 0.000000000000000000 ) ) ;
#10302 = CARTESIAN_POINT ( 'NONE',  ( 16.23204215805303008, 5.269564841427452073, -8.982820748099108243 ) ) ;
#10303 = CARTESIAN_POINT ( 'NONE',  ( -3.000000000000000000, 22.00000000000000000, 0.000000000000000000 ) ) ;
#10304 = DIRECTION ( 'NONE',  ( -1.000000000000000000, 0.000000000000000000, 0.000000000000000000 ) ) ;
#10305 = DIRECTION ( 'NONE',  ( 0.000000000000000000, 0.4098987730065234425, -0.9121310190360518710 ) ) ;
#10306 = ORIENTED_EDGE ( 'NONE', *, *, #10973, .F. ) ;
#10307 = CARTESIAN_POINT ( 'NONE',  ( 61.60588651278290939, 37.01856778792605240, 6.000000000000000000 ) ) ;
#10308 = AXIS2_PLACEMENT_3D ( 'NONE', #13447, #9940, #17204 ) ;
#10309 = CARTESIAN_POINT ( 'NONE',  ( -3.792676939738165220, 12.19816298709897140, -2.925173950252105470 ) ) ;
#10310 = CIRCLE ( 'NONE', #19599, 4.724999999999999645 ) ;
#10311 = VERTEX_POINT ( 'NONE', #9234 ) ;
#10312 = CARTESIAN_POINT ( 'NONE',  ( 1.952358158081999973, 24.36111943012999959, 1.918398575790000171 ) ) ;
#10313 = EDGE_CURVE ( 'NONE', #9228, #12236, #2292, .T. ) ;
#10314 = CARTESIAN_POINT ( 'NONE',  ( 0.000000000000000000, 28.00000000000000000, 4.618802153517000519 ) ) ;
#10315 = CARTESIAN_POINT ( 'NONE',  ( -2.914577979011814257, 13.09053447596949837, 6.080397015720073739 ) ) ;
#10316 = ADVANCED_FACE ( 'NONE', ( #1435 ), #16606, .T. ) ;
#10317 = CARTESIAN_POINT ( 'NONE',  ( 6.185781828581297326, 13.94115629030004833, -0.7324217553683136650 ) ) ;
#10318 = LINE ( 'NONE', #2688, #9815 ) ;
#10319 = DIRECTION ( 'NONE',  ( 0.000000000000000000, -1.000000000000000000, 0.000000000000000000 ) ) ;
#10320 = AXIS2_PLACEMENT_3D ( 'NONE', #22095, #23676, #8797 ) ;
#10321 = VERTEX_POINT ( 'NONE', #23596 ) ;
#10322 = CARTESIAN_POINT ( 'NONE',  ( 0.000000000000000000, 24.39999999221199900, 0.000000000000000000 ) ) ;
#10323 = LINE ( 'NONE', #17339, #91 ) ;
#10324 = CARTESIAN_POINT ( 'NONE',  ( -20.25016455292000117, -8.657612072530000091, 3.085311466348000131 ) ) ;
#10325 = EDGE_LOOP ( 'NONE', ( #5742, #15050, #23007, #2841, #13140 ) ) ;
#10326 = EDGE_CURVE ( 'NONE', #629, #7062, #7111, .T. ) ;
#10327 = CARTESIAN_POINT ( 'NONE',  ( -24.61851251388999984, -10.08336777178000077, -5.147008447691999500 ) ) ;
#10328 = DIRECTION ( 'NONE',  ( 0.000000000000000000, 1.000000000000000000, 0.000000000000000000 ) ) ;
#10329 = CIRCLE ( 'NONE', #23846, 4.000000000000000000 ) ;
#10330 = DIRECTION ( 'NONE',  ( 0.000000000000000000, 0.000000000000000000, -1.000000000000000000 ) ) ;
#10331 = CARTESIAN_POINT ( 'NONE',  ( 14.89611160934172318, 10.30233908782160945, -0.7821794371295839321 ) ) ;
#10332 = CARTESIAN_POINT ( 'NONE',  ( -1.399999855176999874, 6.999999855177000185, 5.700011345002000930E-07 ) ) ;
#10333 = CARTESIAN_POINT ( 'NONE',  ( 2.297600999428000002, 28.79350652947999833, 0.5222559440399000552 ) ) ;
#10334 = FACE_OUTER_BOUND ( 'NONE', #7572, .T. ) ;
#10335 = CARTESIAN_POINT ( 'NONE',  ( -4.741933015551000885, 12.61529762423000456, -0.01097304939024999759 ) ) ;
#10336 = EDGE_LOOP ( 'NONE', ( #3670, #11265 ) ) ;
#10337 = FACE_OUTER_BOUND ( 'NONE', #20142, .T. ) ;
#10338 = CARTESIAN_POINT ( 'NONE',  ( -1.856171584524297202, 29.47206855671609205, 1.104583064503529277 ) ) ;
#10339 = VERTEX_POINT ( 'NONE', #5306 ) ;
#10340 = VECTOR ( 'NONE', #11658, 1000.000000000000227 ) ;
#10341 = CARTESIAN_POINT ( 'NONE',  ( -1.368902347425000166, 23.50118614385000271, -1.908701113743999978 ) ) ;
#10342 = CARTESIAN_POINT ( 'NONE',  ( -17.18329701215404626, 0.2739043995376635454, -10.42461585661749091 ) ) ;
#10343 = VECTOR ( 'NONE', #11145, 1000.000000000000114 ) ;
#10344 = ORIENTED_EDGE ( 'NONE', *, *, #4973, .F. ) ;
#10345 = B_SPLINE_SURFACE_WITH_KNOTS ( 'NONE', 3, 3, ( 
 ( #16117, #5581, #21826, #16708, #5239, #7272, #9454, #3541, #16474, #22059, #20009, #3430, #12624, #9336, #9218, #16597, #18205, #10814, #12850, #8, #5468, #1606, #21940, #1712, #23865, #8991, #120, #16362, #9102, #14431, #14664, #11280, #23751, #13081, #7155 ),
 ( #20246, #3652, #14545, #5350, #12739, #20133, #1950, #11038, #10924, #14890, #18421, #18311, #1832, #7391, #14774, #22170, #12963, #16828, #20359, #3768, #11156, #18542, #7507, #22281, #5696, #20481, #3889, #18657, #2063, #7048, #2302, #8122, #5926, #19252, #17311 ),
 ( #19121, #20952, #22517, #22872, #2176, #13198, #9569, #15009, #2534, #15238, #20591, #15486, #11635, #13310, #18890, #16953, #19003, #17069, #20831, #2663, #7635, #4245, #4357, #18766, #712, #4000, #9688, #9926, #585, #2414, #6289, #11749, #467, #13671, #20708 ),
 ( #9805, #17188, #21065, #4479, #4117, #11868, #354, #10057, #22752, #15122, #13554, #232, #22407, #5816, #22631, #7989, #11396, #15361, #7754, #11515, #7870, #6171, #6042, #13431, #23236, #19380, #21683, #15847, #15605, #5095, #19749, #2791, #3034, #4731, #13792 ) ),
 .UNSPECIFIED., .F., .F., .F.,
 ( 4, 4 ),
 ( 4, 1, 1, 1, 1, 1, 1, 1, 1, 1, 1, 1, 1, 1, 1, 1, 1, 1, 1, 1, 1, 1, 1, 1, 1, 1, 1, 1, 1, 1, 1, 1, 4 ),
 ( -0.3056682515952000023, 1.305668251594999996 ),
 ( -0.01313663885146000056, 0.008210399282161001330, 0.02955743741577999961, 0.05090447554939999536, 0.07225151368301999111, 0.09359855181663999379, 0.1149455899503000061, 0.1362926280838999971, 0.1576396662175000019, 0.1789867043511000066, 0.2003337424846999837, 0.2216807806182999885, 0.2430278187519999966, 0.2643748568855999737, 0.2857218950191999784, 0.3070689331527999832, 0.3284159712863999880, 0.3497630094201000239, 0.3711100475536999732, 0.3924570856872999780, 0.4138041238209000383, 0.4351511619544999876, 0.4564982000882000235, 0.4778452382218000283, 0.4991922763553999776, 0.5205393144889999268, 0.5418863526225999871, 0.5632333907561999364, 0.5845804288899000278, 0.6059274670234999771, 0.6272745051571000374, 0.6486215432906999867, 0.6699685814243000470 ),
 .UNSPECIFIED. ) ;
#10346 = DIRECTION ( 'NONE',  ( 0.000000000000000000, 0.000000000000000000, -1.000000000000000000 ) ) ;
#10347 = CARTESIAN_POINT ( 'NONE',  ( 6.273483391934002285, 13.70231627968000154, 0.06241200954222003022 ) ) ;
#10348 = CARTESIAN_POINT ( 'NONE',  ( 11.99999999999999822, -1.102614627638894174, -8.921479305743723387 ) ) ;
#10349 = CIRCLE ( 'NONE', #11114, 12.50000000000000178 ) ;
#10350 = CARTESIAN_POINT ( 'NONE',  ( 17.50558333333332328, 8.883175614560848032, 2.387156777129599394 ) ) ;
#10351 = CARTESIAN_POINT ( 'NONE',  ( 12.87112658530999987, 8.616207371593000985, 5.326914196072999985 ) ) ;
#10352 = ORIENTED_EDGE ( 'NONE', *, *, #23581, .T. ) ;
#10353 = DIRECTION ( 'NONE',  ( 0.000000000000000000, -1.000000000000000000, 0.000000000000000000 ) ) ;
#10354 = DIRECTION ( 'NONE',  ( 0.000000000000000000, -1.000000000000000000, 0.000000000000000000 ) ) ;
#10355 = DIRECTION ( 'NONE',  ( 0.000000000000000000, 0.000000000000000000, 1.000000000000000000 ) ) ;
#10356 = EDGE_LOOP ( 'NONE', ( #129, #16840, #139, #7848, #18190, #22250, #2015, #6027, #21474, #3465 ) ) ;
#10357 = CARTESIAN_POINT ( 'NONE',  ( 11.06626444616535387, 10.95085460509868369, 6.032555207302821465 ) ) ;
#10358 = CARTESIAN_POINT ( 'NONE',  ( -6.249999999202001000, 16.31160201366999729, 0.9999995866763998764 ) ) ;
#10359 = CARTESIAN_POINT ( 'NONE',  ( -5.588326156475896589, 14.56718056557104468, -4.654699638219854663 ) ) ;
#10360 = CARTESIAN_POINT ( 'NONE',  ( 16.22229514016562035, -1.909916386427916057, -10.18956628747337945 ) ) ;
#10361 = AXIS2_PLACEMENT_3D ( 'NONE', #9444, #9560, #5916 ) ;
#10362 = CARTESIAN_POINT ( 'NONE',  ( 12.00000000000000000, -8.840148123257950630, -4.669854054429479540 ) ) ;
#10363 = CARTESIAN_POINT ( 'NONE',  ( -14.47158023610679756, -11.86027760101404205, 4.457335568564623429 ) ) ;
#10364 = AXIS2_PLACEMENT_3D ( 'NONE', #16206, #1325, #1201 ) ;
#10365 = CARTESIAN_POINT ( 'NONE',  ( -4.049719616303214309, 13.80515179997299313, -4.863490999083110999 ) ) ;
#10366 = ADVANCED_FACE ( 'NONE', ( #22128 ), #14672, .F. ) ;
#10367 = CARTESIAN_POINT ( 'NONE',  ( -1.992339167965410773, 30.25593788753863578, 0.8606820921618728581 ) ) ;
#10368 = ORIENTED_EDGE ( 'NONE', *, *, #13234, .F. ) ;
#10369 = CARTESIAN_POINT ( 'NONE',  ( 22.15953394107999941, -5.779992152541000294, 8.618061788542000556 ) ) ;
#10370 = CARTESIAN_POINT ( 'NONE',  ( 22.99472057969317973, -10.13472181993574495, 3.079891000904835252 ) ) ;
#10371 = CARTESIAN_POINT ( 'NONE',  ( 0.6543697108982093891, 27.66753006952333038, 2.434931691670787490 ) ) ;
#10372 = ORIENTED_EDGE ( 'NONE', *, *, #792, .T. ) ;
#10373 = CARTESIAN_POINT ( 'NONE',  ( -19.73387766488721340, 0.7360098622191569850, 10.46330882142914653 ) ) ;
#10374 = CARTESIAN_POINT ( 'NONE',  ( -14.25243324638999809, -13.93375672974000068, -0.8660254037843999608 ) ) ;
#10375 = CIRCLE ( 'NONE', #19244, 7.000000000000000000 ) ;
#10376 = CARTESIAN_POINT ( 'NONE',  ( 4.946082664740999668, 12.51487189599001759, -0.1133811337498999705 ) ) ;
#10377 = EDGE_LOOP ( 'NONE', ( #5404, #2627, #20565 ) ) ;
#10378 = CARTESIAN_POINT ( 'NONE',  ( -15.22817204324037021, -1.771982936837275924, -10.21894444281640624 ) ) ;
#10379 = CARTESIAN_POINT ( 'NONE',  ( 17.64450125731000085, 9.220888413547999818, -0.5479559280035000146 ) ) ;
#10380 = ORIENTED_EDGE ( 'NONE', *, *, #10564, .T. ) ;
#10381 = CARTESIAN_POINT ( 'NONE',  ( 1.997037326419333070, 27.17506949985559217, 0.9200039467642276980 ) ) ;
#10382 = DIRECTION ( 'NONE',  ( 1.000000000000000000, 0.000000000000000000, 0.000000000000000000 ) ) ;
#10383 = AXIS2_PLACEMENT_3D ( 'NONE', #22757, #6294, #13676 ) ;
#10384 = CARTESIAN_POINT ( 'NONE',  ( -5.194121241778000275, 0.000000000000000000, 0.000000000000000000 ) ) ;
#10385 = EDGE_LOOP ( 'NONE', ( #21477, #9035, #18753, #15813 ) ) ;
#10386 = CARTESIAN_POINT ( 'NONE',  ( -19.30504787661167043, 6.323484023877028015, 6.721981018013264197 ) ) ;
#10387 = CARTESIAN_POINT ( 'NONE',  ( 13.00725174931000083, 10.48226630763000067, 1.840397312871999924 ) ) ;
#10388 = CARTESIAN_POINT ( 'NONE',  ( -14.29555379409998928, -1.242885911923757858, -8.999946461797254216 ) ) ;
#10389 = CARTESIAN_POINT ( 'NONE',  ( -16.84797557115999922, 10.17000433686999905, 3.756487055001000108 ) ) ;
#10390 = CARTESIAN_POINT ( 'NONE',  ( -6.137760362496004873, 15.63629344804000887, 1.260435990244000326 ) ) ;
#10391 = CARTESIAN_POINT ( 'NONE',  ( 16.81806994525999954, 1.942066464734999887, -10.12485589047999923 ) ) ;
#10392 = CARTESIAN_POINT ( 'NONE',  ( 0.4078570127197936324, 28.38048613814547494, -2.134782185931087373 ) ) ;
#10393 = VECTOR ( 'NONE', #16260, 1000.000000000000227 ) ;
#10394 = DIRECTION ( 'NONE',  ( 0.000000000000000000, -1.000000000000000000, 0.000000000000000000 ) ) ;
#10395 = ADVANCED_FACE ( 'NONE', ( #11238 ), #15823, .F. ) ;
#10396 = CARTESIAN_POINT ( 'NONE',  ( 24.48085323735392294, 8.653296529984718433, 5.020612371803464313 ) ) ;
#10397 = ORIENTED_EDGE ( 'NONE', *, *, #12390, .F. ) ;
#10398 = CARTESIAN_POINT ( 'NONE',  ( 2.808569713089370534, 14.07519307301941147, 5.443121979668293697 ) ) ;
#10399 = CARTESIAN_POINT ( 'NONE',  ( -1.932944458086000017, 26.07369850838000147, -1.184521108792000010 ) ) ;
#10400 = LINE ( 'NONE', #14147, #21997 ) ;
#10401 = VECTOR ( 'NONE', #16308, 1000.000000000000000 ) ;
#10402 = CARTESIAN_POINT ( 'NONE',  ( -22.41645255698000128, 10.23964721874999917, -4.326993456033999763 ) ) ;
#10403 = CONICAL_SURFACE ( 'NONE', #3825, 3.049999825846000157, 0.7853981633972997312 ) ;
#10404 = COLOUR_RGB ( '', 0.72549020, 0.75294118, 0.79215686) ;
#10405 = CARTESIAN_POINT ( 'NONE',  ( -4.836653794536299955, 12.44483666031821834, 0.4214316309137807748 ) ) ;
#10406 = ORIENTED_EDGE ( 'NONE', *, *, #22848, .T. ) ;
#10407 = DIRECTION ( 'NONE',  ( 0.000000000000000000, -1.000000000000000000, 0.000000000000000000 ) ) ;
#10408 = CARTESIAN_POINT ( 'NONE',  ( 2.466980964282978750, 11.74073273616931168, -4.142218052624875746 ) ) ;
#10409 = EDGE_CURVE ( 'NONE', #18970, #19401, #18266, .T. ) ;
#10410 = DIRECTION ( 'NONE',  ( 0.000000000000000000, -1.000000000000000000, 0.000000000000000000 ) ) ;
#10411 = AXIS2_PLACEMENT_3D ( 'NONE', #9409, #11797, #16549 ) ;
#10412 = CARTESIAN_POINT ( 'NONE',  ( 6.696152422707000618, 28.00000000000000000, 6.000000000000000000 ) ) ;
#10413 = DIRECTION ( 'NONE',  ( -1.000000000000000000, 0.000000000000000000, 0.000000000000000000 ) ) ;
#10414 = CARTESIAN_POINT ( 'NONE',  ( 12.00000000000000000, -10.65000000000000036, 0.000000000000000000 ) ) ;
#10415 = CARTESIAN_POINT ( 'NONE',  ( -14.05208405859999843, -9.143870435873997948, 6.637879840603000403 ) ) ;
#10416 = CARTESIAN_POINT ( 'NONE',  ( 11.28262625730999957, -8.806575700274999363, 0.9184129047361999643 ) ) ;
#10417 = DIRECTION ( 'NONE',  ( 1.000000000000000000, 0.000000000000000000, 0.000000000000000000 ) ) ;
#10418 = VECTOR ( 'NONE', #21575, 1000.000000000000000 ) ;
#10419 = ORIENTED_EDGE ( 'NONE', *, *, #7616, .F. ) ;
#10420 = CARTESIAN_POINT ( 'NONE',  ( 5.290856909789264151, 13.79953964304391789, 4.259698828153141825 ) ) ;
#10421 = CARTESIAN_POINT ( 'NONE',  ( 2.354726837831999653, 29.90653759481000051, 0.9329478987628000430 ) ) ;
#10422 = CARTESIAN_POINT ( 'NONE',  ( 4.000000000000000000, 24.50000000000000000, 2.309401076759000304 ) ) ;
#10423 = CARTESIAN_POINT ( 'NONE',  ( 2.717593476773952688, 14.04971210407079951, -5.492367343542457370 ) ) ;
#10424 = AXIS2_PLACEMENT_3D ( 'NONE', #20923, #2632, #555 ) ;
#10425 = VERTEX_POINT ( 'NONE', #7225 ) ;
#10426 = DIRECTION ( 'NONE',  ( 0.000000000000000000, 0.000000000000000000, -1.000000000000000000 ) ) ;
#10427 = CARTESIAN_POINT ( 'NONE',  ( -24.50000000000000000, -10.82531754731000007, 6.250000000000000000 ) ) ;
#10428 = EDGE_CURVE ( 'NONE', #13740, #11881, #22787, .T. ) ;
#10429 = CARTESIAN_POINT ( 'NONE',  ( 16.52299999999999969, -9.095294458157999529, 0.000000000000000000 ) ) ;
#10430 = CARTESIAN_POINT ( 'NONE',  ( -23.74465998031000069, -6.216878364870000340, 12.50000000000000000 ) ) ;
#10431 = CARTESIAN_POINT ( 'NONE',  ( 15.86963858528391391, -6.901509964614469972, -7.784720662817159464 ) ) ;
#10432 = CARTESIAN_POINT ( 'NONE',  ( -3.870976219244578242, 13.99445802289816321, 4.846937829204491344 ) ) ;
#10433 = CIRCLE ( 'NONE', #338, 0.5500000000000001554 ) ;
#10434 = DIRECTION ( 'NONE',  ( 0.000000000000000000, -1.000000000000000000, 0.000000000000000000 ) ) ;
#10435 = CYLINDRICAL_SURFACE ( 'NONE', #9634, 3.000000000000000000 ) ;
#10436 = ORIENTED_EDGE ( 'NONE', *, *, #7761, .T. ) ;
#10437 = CARTESIAN_POINT ( 'NONE',  ( -2.500000000000000000, 18.50000000000000000, 0.000000000000000000 ) ) ;
#10438 = CARTESIAN_POINT ( 'NONE',  ( 1.252030728491252409, 11.63101246561627278, -4.623972916844822478 ) ) ;
#10439 = ORIENTED_EDGE ( 'NONE', *, *, #4448, .F. ) ;
#10440 = AXIS2_PLACEMENT_3D ( 'NONE', #5027, #20262, #11053 ) ;
#10441 = CARTESIAN_POINT ( 'NONE',  ( -0.9641736524564000765, 24.60403619718000101, -2.355488194562000093 ) ) ;
#10442 = CARTESIAN_POINT ( 'NONE',  ( 5.509196045612000603, 14.23526548753000576, 2.583477358259002710 ) ) ;
#10443 = EDGE_CURVE ( 'NONE', #889, #12315, #750, .T. ) ;
#10444 = CARTESIAN_POINT ( 'NONE',  ( 1.662687440517862214, 12.89555417843306806, 6.484250417384837206 ) ) ;
#10445 = AXIS2_PLACEMENT_3D ( 'NONE', #6421, #15167, #1097 ) ;
#10446 = CARTESIAN_POINT ( 'NONE',  ( 12.50000000000000000, 13.93375672974000068, 0.1442689875826000112 ) ) ;
#10447 = CARTESIAN_POINT ( 'NONE',  ( -11.00000000000000000, 1.359357947053999856E-14, 0.000000000000000000 ) ) ;
#10448 = CIRCLE ( 'NONE', #23959, 15.43375672974000068 ) ;
#10449 = CARTESIAN_POINT ( 'NONE',  ( -19.10482910584000038, 1.458613477275000161E-14, 0.000000000000000000 ) ) ;
#10450 = ORIENTED_EDGE ( 'NONE', *, *, #11575, .T. ) ;
#10451 = CARTESIAN_POINT ( 'NONE',  ( -3.821520914465098784, 29.74995697614778578, -2.412446024836691461 ) ) ;
#10452 = CARTESIAN_POINT ( 'NONE',  ( -0.4031052425579070286, 26.23085661886908326, 2.096221175781856072 ) ) ;
#10453 = CARTESIAN_POINT ( 'NONE',  ( -10.04281598263999875, 16.43285860070443860, 0.1718092760798937135 ) ) ;
#10454 = ORIENTED_EDGE ( 'NONE', *, *, #23537, .T. ) ;
#10455 = CARTESIAN_POINT ( 'NONE',  ( -22.48958999300999650, -8.088488029599998796, -7.066540705739000394 ) ) ;
#10456 = CARTESIAN_POINT ( 'NONE',  ( 20.64229166666665805, 1.204281607287347011, -9.201003601022879508 ) ) ;
#10457 = CARTESIAN_POINT ( 'NONE',  ( 15.07109509836083383, 8.896268110734828483, 5.261584688652965802 ) ) ;
#10458 = CARTESIAN_POINT ( 'NONE',  ( 4.000000000000000000, 24.50000000000000000, 0.000000000000000000 ) ) ;
#10459 = EDGE_CURVE ( 'NONE', #15241, #20808, #22027, .T. ) ;
#10460 = DIRECTION ( 'NONE',  ( -0.7071067811905932254, -0.7071067811824932603, -1.099460899159990341E-07 ) ) ;
#10461 = CARTESIAN_POINT ( 'NONE',  ( 3.099999776787000005, 20.00000022320933013, 5.570936504208000122E-07 ) ) ;
#10462 = EDGE_CURVE ( 'NONE', #7012, #9517, #2492, .T. ) ;
#10463 = CARTESIAN_POINT ( 'NONE',  ( 4.448835664791996436, 12.50232644074000099, -1.677463259861998290 ) ) ;
#10464 = ORIENTED_EDGE ( 'NONE', *, *, #21768, .F. ) ;
#10465 = CARTESIAN_POINT ( 'NONE',  ( -16.08338753829999845, -2.146827734392999787, 11.15102392286999944 ) ) ;
#10466 = CARTESIAN_POINT ( 'NONE',  ( -1.646340102500975622, 29.31421555423750291, -1.398084700589298457 ) ) ;
#10467 = ORIENTED_EDGE ( 'NONE', *, *, #20180, .F. ) ;
#10468 = FACE_OUTER_BOUND ( 'NONE', #10675, .T. ) ;
#10469 = CARTESIAN_POINT ( 'NONE',  ( -16.14148675361209229, -4.939254558134616779, 9.149695053219954133 ) ) ;
#10470 = VECTOR ( 'NONE', #17258, 1000.000000000000114 ) ;
#10471 = ORIENTED_EDGE ( 'NONE', *, *, #20089, .F. ) ;
#10472 = CARTESIAN_POINT ( 'NONE',  ( 6.171933277826004094, 13.72618630928000627, -1.141834261405999973 ) ) ;
#10473 = EDGE_CURVE ( 'NONE', #1236, #22071, #17496, .T. ) ;
#10474 = CARTESIAN_POINT ( 'NONE',  ( 11.99999999999999822, 2.003559370708953402, -8.770491923202531126 ) ) ;
#10475 = EDGE_CURVE ( 'NONE', #16783, #8124, #5035, .T. ) ;
#10476 = CARTESIAN_POINT ( 'NONE',  ( 14.33221009380999966, 6.651214311818000269, -8.775228328761999208 ) ) ;
#10477 = CARTESIAN_POINT ( 'NONE',  ( 12.32268908530999951, 2.255737295330999981, -9.860771559977997924 ) ) ;
#10478 = VERTEX_POINT ( 'NONE', #9762 ) ;
#10479 = CARTESIAN_POINT ( 'NONE',  ( -9.298203992920999639, -13.92019145675999958, -4.121763198284000396 ) ) ;
#10480 = FACE_OUTER_BOUND ( 'NONE', #8918, .T. ) ;
#10481 = FACE_OUTER_BOUND ( 'NONE', #11774, .T. ) ;
#10482 = VERTEX_POINT ( 'NONE', #22476 ) ;
#10483 = DIRECTION ( 'NONE',  ( 0.000000000000000000, 1.000000000000000000, 0.000000000000000000 ) ) ;
#10484 = CARTESIAN_POINT ( 'NONE',  ( 23.23527882761811014, -3.583123978552704703, -9.970115068474655118 ) ) ;
#10485 = B_SPLINE_CURVE_WITH_KNOTS ( 'NONE', 3,
 ( #21139, #4681, #13506, #10000, #17391, #4554, #10121, #12068, #786, #23786, #8793, #6965, #10727, #23673, #7082, #14357, #21863, #1525, #16155, #7193, #1635, #19815, #23424, #5273 ),
 .UNSPECIFIED., .F., .F.,
 ( 4, 2, 2, 2, 2, 2, 2, 2, 2, 2, 2, 4 ),
 ( 0.000000000000000000, 0.1004975296504320992, 0.2009950593008641706, 0.2512438241260802063, 0.3014925889512962143, 0.4019901186017282302, 0.4522388834269442381, 0.5024876482521603016, 0.6029851779025924285, 0.7034827075530244445, 0.7537314723782405634, 0.8039802372034564604 ),
 .UNSPECIFIED. ) ;
#10486 = DIRECTION ( 'NONE',  ( 0.000000000000000000, 1.000000000000000000, 0.000000000000000000 ) ) ;
#10487 = CARTESIAN_POINT ( 'NONE',  ( 16.80283205072941755, 10.07070901071222124, 2.591683735843758551 ) ) ;
#10488 = CARTESIAN_POINT ( 'NONE',  ( -4.820913537080000033, 13.20111002679000123, 5.836439296936000609 ) ) ;
#10489 = CARTESIAN_POINT ( 'NONE',  ( -14.29262089642102040, -7.983102671798886441, 11.17286057040532832 ) ) ;
#10490 = AXIS2_PLACEMENT_3D ( 'NONE', #1196, #16199, #21305 ) ;
#10491 = CARTESIAN_POINT ( 'NONE',  ( -4.303529988270902606, 13.60822715515925907, -4.961366493816785628 ) ) ;
#10492 = CARTESIAN_POINT ( 'NONE',  ( 0.000000000000000000, 28.00000000000000000, 0.000000000000000000 ) ) ;
#10493 = CARTESIAN_POINT ( 'NONE',  ( -1.921593888566249131, 30.14343111292356880, -0.9863569469920862032 ) ) ;
#10494 = ORIENTED_EDGE ( 'NONE', *, *, #668, .T. ) ;
#10495 = CARTESIAN_POINT ( 'NONE',  ( -1.439810120399000137, 25.29894750743999765, -1.839121480912999873 ) ) ;
#10496 = CARTESIAN_POINT ( 'NONE',  ( 23.95135407356000101, 3.629452715968999765, 10.34366932978999998 ) ) ;
#10497 = CARTESIAN_POINT ( 'NONE',  ( 22.68261335940208312, -2.052889571300259064, 10.38301577081636573 ) ) ;
#10498 = CARTESIAN_POINT ( 'NONE',  ( -2.143277222256999792, 23.64327722226000006, 4.118360636503000477E-13 ) ) ;
#10499 = ORIENTED_EDGE ( 'NONE', *, *, #7194, .T. ) ;
#10500 = FACE_OUTER_BOUND ( 'NONE', #10106, .T. ) ;
#10501 = CARTESIAN_POINT ( 'NONE',  ( 4.978377891991029536, 14.18254257813881125, 3.873879993161618795 ) ) ;
#10502 = B_SPLINE_CURVE_WITH_KNOTS ( 'NONE', 3,
 ( #7141, #1347, #18189, #8973, #23502, #1696, #14530, #5109, #12606, #14305 ),
 .UNSPECIFIED., .F., .F.,
 ( 4, 1, 1, 2, 2, 4 ),
 ( 0.000000000000000000, 0.2499999999999989453, 0.3749999999999988343, 0.4374999999999989453, 0.4999999999999990008, 1.000000000000000000 ),
 .UNSPECIFIED. ) ;
#10503 = CARTESIAN_POINT ( 'NONE',  ( 1.438191898982999151, 11.53459387488998722, -4.742439962699002365 ) ) ;
#10504 = ORIENTED_EDGE ( 'NONE', *, *, #17973, .T. ) ;
#10505 = CARTESIAN_POINT ( 'NONE',  ( -14.72576977311546820, 10.36129416948303827, -0.02468886294351785304 ) ) ;
#10506 = CARTESIAN_POINT ( 'NONE',  ( -12.50000000000000000, 1.557342902441000195E-14, 1.045589212608000028E-14 ) ) ;
#10507 = ORIENTED_EDGE ( 'NONE', *, *, #9354, .T. ) ;
#10508 = B_SPLINE_CURVE_WITH_KNOTS ( 'NONE', 3,
 ( #22251, #5667, #18392, #23960, #7364, #16799, #22145, #4330, #15094, #17416 ),
 .UNSPECIFIED., .F., .F.,
 ( 4, 2, 2, 2, 4 ),
 ( 0.000000000000000000, 0.2499999999999998335, 0.4999999999999996669, 0.7499999999999997780, 1.000000000000000000 ),
 .UNSPECIFIED. ) ;
#10509 = CARTESIAN_POINT ( 'NONE',  ( -12.25000000000000000, -15.45000000000000107, 0.000000000000000000 ) ) ;
#10510 = DIRECTION ( 'NONE',  ( 0.000000000000000000, 0.000000000000000000, 1.000000000000000000 ) ) ;
#10511 = DIRECTION ( 'NONE',  ( -6.780994087986969163E-22, -1.631350558111999873E-10, 1.000000000000000000 ) ) ;
#10512 = VERTEX_POINT ( 'NONE', #306 ) ;
#10513 = CARTESIAN_POINT ( 'NONE',  ( 2.351381211264389925, 26.74999873450825660, 0.9808036171101988110 ) ) ;
#10514 = FACE_OUTER_BOUND ( 'NONE', #9309, .T. ) ;
#10515 = CARTESIAN_POINT ( 'NONE',  ( -24.54530698916000020, 7.467341355790000357, 6.161448972441999850 ) ) ;
#10516 = CARTESIAN_POINT ( 'NONE',  ( -16.64484522318999993, 5.321837195625000128, 9.439042293465000455 ) ) ;
#10517 = FACE_OUTER_BOUND ( 'NONE', #19668, .T. ) ;
#10518 = CARTESIAN_POINT ( 'NONE',  ( 19.52687451746000136, 7.010897399879999270, 6.912477489258999519 ) ) ;
#10519 = CARTESIAN_POINT ( 'NONE',  ( -1.315032585339712234, 27.12168142538949311, 1.729448944228739071 ) ) ;
#10520 = CARTESIAN_POINT ( 'NONE',  ( -7.500000000000000000, 19.50000000000000000, -2.000000000000000000 ) ) ;
#10521 = DIRECTION ( 'NONE',  ( 0.000000000000000000, -1.000000000000000000, 0.000000000000000000 ) ) ;
#10522 = ORIENTED_EDGE ( 'NONE', *, *, #18219, .T. ) ;
#10523 = CARTESIAN_POINT ( 'NONE',  ( -17.72676253787999912, 9.126185377371999863, 0.000000000000000000 ) ) ;
#10524 = CARTESIAN_POINT ( 'NONE',  ( 0.1440416516300269123, 13.69193005210691005, 6.123308775418226269 ) ) ;
#10525 = CARTESIAN_POINT ( 'NONE',  ( 2.266578917753999889, 27.34119850838000332, 0.04450989311242999763 ) ) ;
#10526 = CARTESIAN_POINT ( 'NONE',  ( 0.000000000000000000, 23.75000000000000000, 0.000000000000000000 ) ) ;
#10527 = B_SPLINE_CURVE_WITH_KNOTS ( 'NONE', 3,
 ( #19437, #15656, #22808, #9863, #17248, #13606, #4537, #13489, #2847, #18946 ),
 .UNSPECIFIED., .F., .F.,
 ( 4, 1, 1, 2, 2, 4 ),
 ( 0.000000000000000000, 0.2499999999999989453, 0.3749999999999988343, 0.4374999999999989453, 0.4999999999999990008, 1.000000000000000000 ),
 .UNSPECIFIED. ) ;
#10528 = CARTESIAN_POINT ( 'NONE',  ( -19.42939368183000326, -10.43529125724999851, -0.1440759689522999876 ) ) ;
#10529 = CARTESIAN_POINT ( 'NONE',  ( -4.797719810903769755, 12.43002135603972924, 0.7136055140974607580 ) ) ;
#10530 = VERTEX_POINT ( 'NONE', #15080 ) ;
#10531 = CARTESIAN_POINT ( 'NONE',  ( 4.129449150923196754, 12.19149479092433452, -2.525021771999871767 ) ) ;
#10532 = CARTESIAN_POINT ( 'NONE',  ( 1.716345169325534714, 6.991441436340903870, 0.3950169913663518217 ) ) ;
#10533 = EDGE_LOOP ( 'NONE', ( #5195, #5942, #10834, #8735, #16070 ) ) ;
#10534 = EDGE_CURVE ( 'NONE', #15169, #4052, #19724, .T. ) ;
#10535 = CARTESIAN_POINT ( 'NONE',  ( -24.12232999016000079, 1.520060141252000183E-14, 0.000000000000000000 ) ) ;
#10536 = CARTESIAN_POINT ( 'NONE',  ( -13.23956266673000037, 6.512279107760999608, -9.204720484723999618 ) ) ;
#10537 = CARTESIAN_POINT ( 'NONE',  ( 17.12250142130999819, -8.875724825267999663, -3.992994992864999926 ) ) ;
#10538 = CARTESIAN_POINT ( 'NONE',  ( 18.48965437448689997, 10.24410807905043619, -1.935809810652562524 ) ) ;
#10539 = ORIENTED_EDGE ( 'NONE', *, *, #13816, .F. ) ;
#10540 = CARTESIAN_POINT ( 'NONE',  ( 2.434931691670788823, 28.43333333333332646, -0.6543697108982009514 ) ) ;
#10541 = CARTESIAN_POINT ( 'NONE',  ( 2.309445831590999809, 30.70069424050999984, 1.039994766367999812 ) ) ;
#10542 = DIRECTION ( 'NONE',  ( 0.5882164119205371966, 0.8087035629619353516, -9.903762298403940582E-17 ) ) ;
#10543 = CARTESIAN_POINT ( 'NONE',  ( 4.050551734779913815, 14.47883186787076504, -4.594425583402780511 ) ) ;
#10544 = ORIENTED_EDGE ( 'NONE', *, *, #16904, .F. ) ;
#10545 = FACE_OUTER_BOUND ( 'NONE', #8003, .T. ) ;
#10546 = CYLINDRICAL_SURFACE ( 'NONE', #18176, 14.43375672974000068 ) ;
#10547 = CARTESIAN_POINT ( 'NONE',  ( 0.000000000000000000, 26.35000000000000142, 0.000000000000000000 ) ) ;
#10548 = EDGE_CURVE ( 'NONE', #2693, #19347, #17395, .T. ) ;
#10549 = DIRECTION ( 'NONE',  ( -0.7071067811865474617, -0.7071067811865474617, 0.000000000000000000 ) ) ;
#10550 = CARTESIAN_POINT ( 'NONE',  ( 15.95327017899941069, -4.391970926654074070, -9.430978196784264966 ) ) ;
#10551 = CARTESIAN_POINT ( 'NONE',  ( -7.834000000000000519, 1.320585629393000037E-14, 0.000000000000000000 ) ) ;
#10552 = CARTESIAN_POINT ( 'NONE',  ( 0.000000000000000000, 20.10000000000000142, 0.000000000000000000 ) ) ;
#10553 = DIRECTION ( 'NONE',  ( 1.000000000000000000, 0.000000000000000000, 0.000000000000000000 ) ) ;
#10554 = ORIENTED_EDGE ( 'NONE', *, *, #23442, .T. ) ;
#10555 = CARTESIAN_POINT ( 'NONE',  ( -18.99854661335000117, -13.93375672974000068, 0.000000000000000000 ) ) ;
#10556 = DIRECTION ( 'NONE',  ( -1.734723475976817507E-14, 1.000000000000000000, 1.792956356300015483E-10 ) ) ;
#10557 = VERTEX_POINT ( 'NONE', #17149 ) ;
#10558 = CARTESIAN_POINT ( 'NONE',  ( 1.044258846366000082, 25.30073899244000302, -2.321094337967000154 ) ) ;
#10559 = FACE_OUTER_BOUND ( 'NONE', #18346, .T. ) ;
#10560 = CARTESIAN_POINT ( 'NONE',  ( 5.048184257089419980, 13.64448757289546066, 4.715755534370476454 ) ) ;
#10561 = AXIS2_PLACEMENT_3D ( 'NONE', #12141, #8264, #15511 ) ;
#10562 = CARTESIAN_POINT ( 'NONE',  ( 15.90028936713000185, 9.079314476020000413, 0.000000000000000000 ) ) ;
#10563 = CARTESIAN_POINT ( 'NONE',  ( 1.999167105995449889, 27.68333333333333357, -1.536366799937288086 ) ) ;
#10564 = EDGE_CURVE ( 'NONE', #19119, #18819, #5361, .T. ) ;
#10565 = CARTESIAN_POINT ( 'NONE',  ( -1.686459531786994148, 23.77333333333334764, -1.586187310772563697 ) ) ;
#10566 = ORIENTED_EDGE ( 'NONE', *, *, #20786, .T. ) ;
#10567 = CARTESIAN_POINT ( 'NONE',  ( -3.560623727957783924, 29.81534065533141131, -2.563075085697513078 ) ) ;
#10568 = CARTESIAN_POINT ( 'NONE',  ( 24.24531177150999994, 13.23032192316000000, 0.000000000000000000 ) ) ;
#10569 = CARTESIAN_POINT ( 'NONE',  ( -6.250000000003000267, 15.09565008225999883, -3.212814891752000079 ) ) ;
#10570 = ORIENTED_EDGE ( 'NONE', *, *, #11615, .T. ) ;
#10571 = CARTESIAN_POINT ( 'NONE',  ( -20.70340094334000014, -9.917170701048998893, 2.249121287463999863 ) ) ;
#10572 = DIRECTION ( 'NONE',  ( 0.000000000000000000, 1.000000000000000000, 0.000000000000000000 ) ) ;
#10573 = CARTESIAN_POINT ( 'NONE',  ( 15.15542662814268304, 7.010537146779027395, 7.597953863240286765 ) ) ;
#10574 = DIRECTION ( 'NONE',  ( 0.000000000000000000, 1.000000000000000000, 0.000000000000000000 ) ) ;
#10575 = CARTESIAN_POINT ( 'NONE',  ( -0.8039427155937000080, 29.93886808515000197, -2.013420029665999866 ) ) ;
#10576 = EDGE_CURVE ( 'NONE', #3964, #20732, #3491, .T. ) ;
#10577 = DIRECTION ( 'NONE',  ( -1.000000000000000000, 0.000000000000000000, 0.000000000000000000 ) ) ;
#10578 = CARTESIAN_POINT ( 'NONE',  ( 3.724578230166001980, 12.24861053738000294, -2.969015338948001848 ) ) ;
#10579 = ORIENTED_EDGE ( 'NONE', *, *, #6010, .T. ) ;
#10580 = CONICAL_SURFACE ( 'NONE', #15175, 2.249999993279999888, 0.7853981633972997312 ) ;
#10581 = CARTESIAN_POINT ( 'NONE',  ( -8.250000000000000000, 20.24999999999999645, -1.000000000000000000 ) ) ;
#10582 = ORIENTED_EDGE ( 'NONE', *, *, #10534, .F. ) ;
#10583 = CARTESIAN_POINT ( 'NONE',  ( -0.6543697108982037269, 29.43333333333334068, -2.434931691670788823 ) ) ;
#10584 = CARTESIAN_POINT ( 'NONE',  ( 0.000000000000000000, -1.550000000000000044, 0.000000000000000000 ) ) ;
#10585 = ADVANCED_FACE ( 'NONE', ( #793 ), #427, .T. ) ;
#10586 = ORIENTED_EDGE ( 'NONE', *, *, #10005, .F. ) ;
#10587 = CARTESIAN_POINT ( 'NONE',  ( 11.83261479513038061, -13.04738324255308690, -2.401298039148104024 ) ) ;
#10588 = CARTESIAN_POINT ( 'NONE',  ( -4.772366215095780184, 13.34838505587969948, -5.491644434773237826 ) ) ;
#10589 = B_SPLINE_CURVE_WITH_KNOTS ( 'NONE', 3,
 ( #2975, #4678, #12063, #19449, #17630 ),
 .UNSPECIFIED., .F., .F.,
 ( 4, 1, 4 ),
 ( 0.000000000000000000, 0.5000000000000000000, 1.000000000000000000 ),
 .UNSPECIFIED. ) ;
#10590 = CARTESIAN_POINT ( 'NONE',  ( 16.31716997010999748, 10.46811184600000111, -3.586373476968000240 ) ) ;
#10591 = ADVANCED_FACE ( 'NONE', ( #7950 ), #4077, .F. ) ;
#10592 = CARTESIAN_POINT ( 'NONE',  ( 2.467893978438000069, 27.18256359724000149, 0.04846321314148000631 ) ) ;
#10593 = CARTESIAN_POINT ( 'NONE',  ( 11.99362658531000037, -8.009633343651000104, -6.163949985837000156 ) ) ;
#10594 = EDGE_CURVE ( 'NONE', #2374, #13175, #9136, .T. ) ;
#10595 = EDGE_LOOP ( 'NONE', ( #4604, #971, #16486, #19649, #11900 ) ) ;
#10596 = DIRECTION ( 'NONE',  ( 0.000000000000000000, -1.000000000000000000, 0.000000000000000000 ) ) ;
#10597 = CARTESIAN_POINT ( 'NONE',  ( 13.50000000000000000, 9.162136282950783084, -2.282264667262656310 ) ) ;
#10598 = DIRECTION ( 'NONE',  ( -1.000000000000000000, 0.000000000000000000, 0.000000000000000000 ) ) ;
#10599 = EDGE_LOOP ( 'NONE', ( #7802, #1449, #20079, #10566, #22215, #19137 ) ) ;
#10600 = CARTESIAN_POINT ( 'NONE',  ( -23.20138028387000162, 9.293596334485000554, -2.826991214650000028 ) ) ;
#10601 = CARTESIAN_POINT ( 'NONE',  ( 11.39490977864433141, 12.26833003003861933, 3.750544030113681426 ) ) ;
#10602 = CARTESIAN_POINT ( 'NONE',  ( 21.20567237728856824, -9.515960249491415723, -4.901612566710888963 ) ) ;
#10603 = VECTOR ( 'NONE', #5866, 1000.000000000000000 ) ;
#10604 = CARTESIAN_POINT ( 'NONE',  ( -5.420127902049621582, 15.54531213489060981, 2.854267850004046814 ) ) ;
#10605 = CARTESIAN_POINT ( 'NONE',  ( 16.19937828008823644, -2.727843005219428019, -9.999616570623473422 ) ) ;
#10606 = DIRECTION ( 'NONE',  ( -1.000000000000000000, 0.000000000000000000, 0.000000000000000000 ) ) ;
#10607 = CARTESIAN_POINT ( 'NONE',  ( -2.009419033758999884, 29.34560438995000098, -1.204887936538999949 ) ) ;
#10608 = EDGE_CURVE ( 'NONE', #19829, #11381, #2251, .T. ) ;
#10609 = EDGE_CURVE ( 'NONE', #13196, #3216, #16328, .T. ) ;
#10610 = CARTESIAN_POINT ( 'NONE',  ( 1.346994075275769864, 29.91795814813315957, -1.688431679418926912 ) ) ;
#10611 = ORIENTED_EDGE ( 'NONE', *, *, #66, .F. ) ;
#10612 = CARTESIAN_POINT ( 'NONE',  ( 21.87815553483999764, 9.951306365835000278, -5.643451686609999740 ) ) ;
#10613 = CARTESIAN_POINT ( 'NONE',  ( 24.35664299550522927, 3.038500614219330931, 10.17926622196943498 ) ) ;
#10614 = DIRECTION ( 'NONE',  ( -0.5000000000000169864, 0.000000000000000000, 0.8660254037844289376 ) ) ;
#10615 = VECTOR ( 'NONE', #19648, 1000.000000000000000 ) ;
#10616 = VERTEX_POINT ( 'NONE', #6849 ) ;
#10617 = DIRECTION ( 'NONE',  ( 0.000000000000000000, 0.000000000000000000, -1.000000000000000000 ) ) ;
#10618 = CARTESIAN_POINT ( 'NONE',  ( 4.893783511618616799, 14.39890544002889428, -3.811344258107727256 ) ) ;
#10619 = CARTESIAN_POINT ( 'NONE',  ( -3.300528186783000084, 11.98006166429998665, -3.696077710035002628 ) ) ;
#10620 = ORIENTED_EDGE ( 'NONE', *, *, #6581, .T. ) ;
#10621 = CARTESIAN_POINT ( 'NONE',  ( 17.31543875730999815, 3.351454173900000111, -8.598433847594998625 ) ) ;
#10622 = VECTOR ( 'NONE', #15874, 1000.000000000000000 ) ;
#10623 = AXIS2_PLACEMENT_3D ( 'NONE', #5977, #8168, #2350 ) ;
#10624 = ORIENTED_EDGE ( 'NONE', *, *, #12498, .F. ) ;
#10625 = CARTESIAN_POINT ( 'NONE',  ( 22.83443279375291368, 36.19190089707605296, -6.000000000000000000 ) ) ;
#10626 = DIRECTION ( 'NONE',  ( 0.000000000000000000, -1.000000000000000000, 0.000000000000000000 ) ) ;
#10627 = ORIENTED_EDGE ( 'NONE', *, *, #15777, .F. ) ;
#10628 = CARTESIAN_POINT ( 'NONE',  ( 11.00000000000000000, -10.59999999999999964, 0.000000000000000000 ) ) ;
#10629 = CARTESIAN_POINT ( 'NONE',  ( 12.34912674931000076, -5.416870430593999863, -9.140812312194999123 ) ) ;
#10630 = CARTESIAN_POINT ( 'NONE',  ( -23.63377946391999984, -9.915102125873000105, 2.288295221134000190 ) ) ;
#10631 = CARTESIAN_POINT ( 'NONE',  ( 11.43887872962712038, -9.287405149881228894, -8.913622445545286155 ) ) ;
#10633 = EDGE_CURVE ( 'NONE', #19401, #1045, #20120, .T. ) ;
#10632 = CARTESIAN_POINT ( 'NONE',  ( -4.939568633879000359, 13.53408867494998802, -5.800137320629999316 ) ) ;
#10634 = CARTESIAN_POINT ( 'NONE',  ( -24.21590912748918711, 7.621690869234290844, -7.366582963188160527 ) ) ;
#10635 = CARTESIAN_POINT ( 'NONE',  ( -1.015900767931854354, 27.66495503860647887, -1.959239081289818385 ) ) ;
#10636 = DIRECTION ( 'NONE',  ( 0.000000000000000000, 0.000000000000000000, 1.000000000000000000 ) ) ;
#10637 = CARTESIAN_POINT ( 'NONE',  ( 14.86016666666666808, -7.910107230074322260, -4.558955418934749204 ) ) ;
#10638 = ORIENTED_EDGE ( 'NONE', *, *, #8515, .T. ) ;
#10639 = CARTESIAN_POINT ( 'NONE',  ( -17.34884587121334221, 2.386103976833011231, 8.879258109265995458 ) ) ;
#10640 = CARTESIAN_POINT ( 'NONE',  ( 3.918815203773234224, 14.42969747532489677, 4.707339579678993857 ) ) ;
#10641 = CARTESIAN_POINT ( 'NONE',  ( -0.5696873960579796892, 24.75754694542404621, 2.081016722391946239 ) ) ;
#10642 = DIRECTION ( 'NONE',  ( 0.8947368421052591669, 0.000000000000000000, 0.4465937565388801156 ) ) ;
#10643 = FACE_OUTER_BOUND ( 'NONE', #8339, .T. ) ;
#10644 = AXIS2_PLACEMENT_3D ( 'NONE', #10437, #17827, #6786 ) ;
#10645 = CARTESIAN_POINT ( 'NONE',  ( -4.313940323335201832, 12.25428752138464361, 2.199116708544083476 ) ) ;
#10646 = VERTEX_POINT ( 'NONE', #15804 ) ;
#10647 = CYLINDRICAL_SURFACE ( 'NONE', #5296, 2.500000000000000000 ) ;
#10648 = CARTESIAN_POINT ( 'NONE',  ( 2.929890266377786379, 11.84452384940898284, -3.836082332777877912 ) ) ;
#10649 = VECTOR ( 'NONE', #10822, 1000.000000000000114 ) ;
#10650 = CARTESIAN_POINT ( 'NONE',  ( 11.55866343642402683, -7.053686836476363631, -5.580721502645149990 ) ) ;
#10651 = ORIENTED_EDGE ( 'NONE', *, *, #2028, .F. ) ;
#10652 = CARTESIAN_POINT ( 'NONE',  ( 0.000000000000000000, -1.550000000000000044, 0.000000000000000000 ) ) ;
#10653 = CARTESIAN_POINT ( 'NONE',  ( -2.399999988616999591, 28.00000001138332806, -6.337991255853999810E-08 ) ) ;
#10654 = CARTESIAN_POINT ( 'NONE',  ( 15.36750142131000096, -7.843339156370999099, -5.684071587432000250 ) ) ;
#10655 = CARTESIAN_POINT ( 'NONE',  ( 18.64504799222103415, 9.813939602435103993, 3.576112584041952314 ) ) ;
#10656 = ORIENTED_EDGE ( 'NONE', *, *, #13260, .T. ) ;
#10657 = CARTESIAN_POINT ( 'NONE',  ( 1.999167105995449889, 28.48333333333334139, -1.536366799937288086 ) ) ;
#10658 = CARTESIAN_POINT ( 'NONE',  ( -0.9058703646527999087, 29.70799843338999935, 2.365275701699999900 ) ) ;
#10659 = CARTESIAN_POINT ( 'NONE',  ( 0.000000000000000000, 28.30000000000000071, -4.618802153517000519 ) ) ;
#10660 = CARTESIAN_POINT ( 'NONE',  ( 13.50000000000000000, -9.675600895433166926, 0.1311100501057143597 ) ) ;
#10661 = AXIS2_PLACEMENT_3D ( 'NONE', #9571, #16477, #11159 ) ;
#10662 = ORIENTED_EDGE ( 'NONE', *, *, #18855, .T. ) ;
#10663 = DIRECTION ( 'NONE',  ( 1.000000000000000000, 0.000000000000000000, 0.000000000000000000 ) ) ;
#10664 = CARTESIAN_POINT ( 'NONE',  ( -24.27585716844503594, -12.49018833526878147, 3.366221553749007445 ) ) ;
#10665 = CARTESIAN_POINT ( 'NONE',  ( 16.22066666666666279, -4.576538324501929544, 7.940613831594722782 ) ) ;
#10666 = CARTESIAN_POINT ( 'NONE',  ( -23.86746844839299797, -5.192331206338657523, 8.183175371501549833 ) ) ;
#10667 = CARTESIAN_POINT ( 'NONE',  ( -24.50000000000000000, -14.43375672974000068, 0.000000000000000000 ) ) ;
#10668 = CARTESIAN_POINT ( 'NONE',  ( -2.327192509895188000, 24.50639765414752347, 3.274853329251978362 ) ) ;
#10669 = CARTESIAN_POINT ( 'NONE',  ( -4.889513280961001129, 12.49342386908999281, 0.7528201520557004089 ) ) ;
#10670 = ADVANCED_FACE ( 'NONE', ( #6613 ), #5056, .F. ) ;
#10671 = DIRECTION ( 'NONE',  ( 0.000000000000000000, 1.000000000000000000, 0.000000000000000000 ) ) ;
#10672 = EDGE_LOOP ( 'NONE', ( #13654, #465, #9714, #22083 ) ) ;
#10673 = CARTESIAN_POINT ( 'NONE',  ( 2.204045812699286344, 30.65849365117777481, 0.9160123963385377044 ) ) ;
#10674 = CARTESIAN_POINT ( 'NONE',  ( 1.724026015792058830, 12.96510883726990038, 1.060380412480157686 ) ) ;
#10675 = EDGE_LOOP ( 'NONE', ( #2330, #12976, #21051 ) ) ;
#10676 = CARTESIAN_POINT ( 'NONE',  ( 2.417770443646000356, 24.39502535860999899, -0.7951990710235999904 ) ) ;
#10677 = DIRECTION ( 'NONE',  ( 0.5000000000000169864, 0.000000000000000000, 0.8660254037844288266 ) ) ;
#10678 = AXIS2_PLACEMENT_3D ( 'NONE', #1391, #10486, #16145 ) ;
#10679 = CARTESIAN_POINT ( 'NONE',  ( 5.302309868036999774, 13.73032359673999814, 4.450989051274000019 ) ) ;
#10680 = CONICAL_SURFACE ( 'NONE', #11825, 9.152445778720998959, 0.02565634000431304615 ) ;
#10681 = CARTESIAN_POINT ( 'NONE',  ( 6.195977518297981490, 13.89472266009280332, -0.8605928538500070557 ) ) ;
#10682 = CARTESIAN_POINT ( 'NONE',  ( 0.000000000000000000, 28.15000000000000213, 0.000000000000000000 ) ) ;
#10683 = ORIENTED_EDGE ( 'NONE', *, *, #15585, .F. ) ;
#10684 = CARTESIAN_POINT ( 'NONE',  ( -14.00000000000000000, -9.461855175648539173, -3.635004795172248393 ) ) ;
#10685 = DIRECTION ( 'NONE',  ( -0.000000000000000000, 1.000000000000000000, -0.000000000000000000 ) ) ;
#10686 = CYLINDRICAL_SURFACE ( 'NONE', #9825, 3.000000000000000000 ) ;
#10687 = ORIENTED_EDGE ( 'NONE', *, *, #8171, .T. ) ;
#10688 = CARTESIAN_POINT ( 'NONE',  ( -19.67520052968999877, 9.945309867329999776, 1.982757173051000077 ) ) ;
#10689 = DIRECTION ( 'NONE',  ( 0.000000000000000000, 1.000000000000000000, 0.000000000000000000 ) ) ;
#10690 = CARTESIAN_POINT ( 'NONE',  ( 14.65641172841788631, 6.408862456806628138, -8.094750487372301961 ) ) ;
#10691 = FACE_OUTER_BOUND ( 'NONE', #2217, .T. ) ;
#10692 = CARTESIAN_POINT ( 'NONE',  ( 24.63960826817999816, -10.15308605020999977, 2.981009416082999852 ) ) ;
#10693 = CARTESIAN_POINT ( 'NONE',  ( -2.146043429168999594, 30.87238359794000075, -0.3073092761724999789 ) ) ;
#10694 = CARTESIAN_POINT ( 'NONE',  ( -22.90514205544799253, 5.691906622003466865, 7.406426240607752121 ) ) ;
#10695 = CARTESIAN_POINT ( 'NONE',  ( -4.722378179075000126, 12.45689350211999979, -0.7786282501865993133 ) ) ;
#10696 = ORIENTED_EDGE ( 'NONE', *, *, #4203, .T. ) ;
#10697 = TOROIDAL_SURFACE ( 'NONE', #7964, 14.44999999999999929, 2.000000000000000000 ) ;
#10698 = CARTESIAN_POINT ( 'NONE',  ( -1.317207735313150607, 26.42011321481863106, 1.933357710794660012 ) ) ;
#10699 = EDGE_CURVE ( 'NONE', #15235, #11532, #23194, .T. ) ;
#10700 = ORIENTED_EDGE ( 'NONE', *, *, #19465, .T. ) ;
#10701 = CARTESIAN_POINT ( 'NONE',  ( -2.500000000000000444, 29.58333333333333925, -0.3272492347489320275 ) ) ;
#10702 = CARTESIAN_POINT ( 'NONE',  ( -14.28937962731940559, -6.103406805596817364, 8.356759130325041696 ) ) ;
#10703 = ORIENTED_EDGE ( 'NONE', *, *, #15327, .F. ) ;
#10704 = CARTESIAN_POINT ( 'NONE',  ( 12.28022044528328038, -13.65679895893291196, -1.345730334378181903 ) ) ;
#10705 = DIRECTION ( 'NONE',  ( 0.000000000000000000, -1.000000000000000000, 0.000000000000000000 ) ) ;
#10706 = CARTESIAN_POINT ( 'NONE',  ( 24.35625626386771003, 3.237027092069015843, -12.49999999999999822 ) ) ;
#10707 = B_SPLINE_CURVE_WITH_KNOTS ( 'NONE', 3,
 ( #9994, #655, #19447, #899, #13986, #11694, #21267, #15550, #19068, #11942 ),
 .UNSPECIFIED., .F., .F.,
 ( 4, 1, 1, 2, 2, 4 ),
 ( 0.000000000000000000, 0.2499999999999969469, 0.3749999999999960032, 0.4374999999999962252, 0.4999999999999963363, 1.000000000000000000 ),
 .UNSPECIFIED. ) ;
#10708 = ADVANCED_FACE ( 'NONE', ( #17887 ), #19282, .T. ) ;
#10709 = VERTEX_POINT ( 'NONE', #126 ) ;
#10710 = AXIS2_PLACEMENT_3D ( 'NONE', #14390, #8340, #13906 ) ;
#10711 = CARTESIAN_POINT ( 'NONE',  ( -10.31642899291999882, 9.736743735031000213, -10.76830904284000034 ) ) ;
#10712 = CIRCLE ( 'NONE', #17657, 12.44999999999999929 ) ;
#10713 = CARTESIAN_POINT ( 'NONE',  ( 13.50000000000000000, 4.517872873748999929, -7.804362139085999850 ) ) ;
#10714 = PLANE ( 'NONE',  #6711 ) ;
#10715 = VERTEX_POINT ( 'NONE', #7161 ) ;
#10716 = CARTESIAN_POINT ( 'NONE',  ( 23.02937672396094371, -9.233243326448210553, -5.186586685900737237 ) ) ;
#10717 = CARTESIAN_POINT ( 'NONE',  ( -14.00000000000000533, 7.443612114797377721, 5.400680299557988562 ) ) ;
#10718 = CARTESIAN_POINT ( 'NONE',  ( 17.07981319014894694, 3.655019374395102716, 9.752800675042001544 ) ) ;
#10719 = EDGE_CURVE ( 'NONE', #12251, #8738, #23134, .T. ) ;
#10720 = CARTESIAN_POINT ( 'NONE',  ( -18.08550596641000396, 9.682332165709999217, 5.434252367816999829 ) ) ;
#10721 = CARTESIAN_POINT ( 'NONE',  ( -1.052033064323999900, 29.27366736927999824, -2.093500996029999506 ) ) ;
#10722 = AXIS2_PLACEMENT_3D ( 'NONE', #19933, #5164, #5505 ) ;
#10723 = CARTESIAN_POINT ( 'NONE',  ( -13.92980981492000048, 8.913287911097999228, 3.799313832512000388 ) ) ;
#10724 = ADVANCED_FACE ( 'NONE', ( #12969 ), #3896, .T. ) ;
#10725 = CARTESIAN_POINT ( 'NONE',  ( 0.5984287563357140183, 29.96812122538106138, -2.076360886265356420 ) ) ;
#10726 = ORIENTED_EDGE ( 'NONE', *, *, #17121, .F. ) ;
#10727 = CARTESIAN_POINT ( 'NONE',  ( 23.36219854623860925, -1.214243892273371817, 9.213288387738314711 ) ) ;
#10728 = CARTESIAN_POINT ( 'NONE',  ( 20.13889713280000038, 11.01791241213000028, -2.895620158417999690 ) ) ;
#10729 = CARTESIAN_POINT ( 'NONE',  ( 19.84527499312657639, -2.175409197760720836, -10.28494925254862480 ) ) ;
#10730 = CIRCLE ( 'NONE', #13801, 2.000000000000000000 ) ;
#10731 = DIRECTION ( 'NONE',  ( 0.000000000000000000, -1.000000000000000000, 0.000000000000000000 ) ) ;
#10732 = VERTEX_POINT ( 'NONE', #9110 ) ;
#10733 = CARTESIAN_POINT ( 'NONE',  ( 0.000000000000000000, 26.50000000000000355, 0.000000000000000000 ) ) ;
#10734 = CARTESIAN_POINT ( 'NONE',  ( 4.846430159580084052, 14.59246997775862908, -3.777182888792198323 ) ) ;
#10735 = CARTESIAN_POINT ( 'NONE',  ( -4.911774959493002690, 12.43823275897999636, 0.1548668838414998805 ) ) ;
#10736 = ORIENTED_EDGE ( 'NONE', *, *, #5666, .T. ) ;
#10737 = EDGE_CURVE ( 'NONE', #3633, #11775, #20450, .T. ) ;
#10738 = CARTESIAN_POINT ( 'NONE',  ( 17.42512625730999787, 6.303186173173999762, -6.744507379544999459 ) ) ;
#10739 = ORIENTED_EDGE ( 'NONE', *, *, #21364, .T. ) ;
#10740 = TOROIDAL_SURFACE ( 'NONE', #13813, 9.651424765286998664, 0.1000000000000000056 ) ;
#10741 = CARTESIAN_POINT ( 'NONE',  ( 2.072318791391040360, 26.38608990294597945, 0.7342227717574281165 ) ) ;
#10742 = CARTESIAN_POINT ( 'NONE',  ( -23.75083293559999831, -13.93375672974000068, -0.6735967306123999965 ) ) ;
#10743 = ORIENTED_EDGE ( 'NONE', *, *, #15869, .F. ) ;
#10744 = CIRCLE ( 'NONE', #16132, 2.399999999999999911 ) ;
#10745 = CARTESIAN_POINT ( 'NONE',  ( -0.006385721344668345532, 26.59999493803301007, 2.547730079617255505 ) ) ;
#10746 = CARTESIAN_POINT ( 'NONE',  ( -21.86732592927000240, -9.361678282808000517, 3.864640653608000243 ) ) ;
#10747 = AXIS2_PLACEMENT_3D ( 'NONE', #2626, #10018, #9653 ) ;
#10748 = CARTESIAN_POINT ( 'NONE',  ( -14.00083134239000060, 8.121744576791000370, -4.249165445770000105 ) ) ;
#10749 = CARTESIAN_POINT ( 'NONE',  ( 0.000000000000000000, 15.00000000000000000, 0.000000000000000000 ) ) ;
#10750 = CARTESIAN_POINT ( 'NONE',  ( -22.67180158262788936, -1.394108788844021118, -10.47118158913528241 ) ) ;
#10751 = CARTESIAN_POINT ( 'NONE',  ( 1.053167012274741410, 27.26743776069429259, 1.938163248592302379 ) ) ;
#10752 = B_SPLINE_CURVE_WITH_KNOTS ( 'NONE', 3,
 ( #9235, #18098, #5597, #14682, #18326, #7064, #23768, #14561, #21957, #7408, #14789, #12639, #22184, #12979, #18562, #1966, #3786, #11175 ),
 .UNSPECIFIED., .F., .F.,
 ( 4, 2, 2, 2, 2, 2, 2, 2, 4 ),
 ( 0.000000000000000000, 0.1250000000000000000, 0.2500000000000000000, 0.3749999999999999445, 0.4999999999999999445, 0.6250000000000000000, 0.7500000000000000000, 0.8750000000000000000, 1.000000000000000000 ),
 .UNSPECIFIED. ) ;
#10753 = CARTESIAN_POINT ( 'NONE',  ( 2.108296854627000005, 27.75500240010000041, -1.948889566018999986 ) ) ;
#10754 = ADVANCED_FACE ( 'NONE', ( #14552 ), #15791, .T. ) ;
#10755 = DIRECTION ( 'NONE',  ( 0.000000000000000000, -1.000000000000000000, 0.000000000000000000 ) ) ;
#10756 = ORIENTED_EDGE ( 'NONE', *, *, #11724, .T. ) ;
#10757 = EDGE_CURVE ( 'NONE', #8812, #23948, #20139, .T. ) ;
#10758 = CARTESIAN_POINT ( 'NONE',  ( 0.000000000000000000, 26.50000000000000000, 0.000000000000000000 ) ) ;
#10759 = CARTESIAN_POINT ( 'NONE',  ( 0.000000000000000000, -1.550000000000000044, 0.000000000000000000 ) ) ;
#10760 = CARTESIAN_POINT ( 'NONE',  ( 0.1334610483750000021, 27.53619850838000360, -2.263084017374999757 ) ) ;
#10761 = CIRCLE ( 'NONE', #2617, 4.750000000000000000 ) ;
#10762 = CIRCLE ( 'NONE', #23105, 12.44999999999999929 ) ;
#10763 = LINE ( 'NONE', #14615, #21892 ) ;
#10764 = CARTESIAN_POINT ( 'NONE',  ( -1.485816803342000281, 27.72271896306000016, -1.739667959131000030 ) ) ;
#10765 = CARTESIAN_POINT ( 'NONE',  ( 0.9483885206027318215, 11.52112569081479698, 4.718712483813342295 ) ) ;
#10766 = ORIENTED_EDGE ( 'NONE', *, *, #6971, .T. ) ;
#10767 = CARTESIAN_POINT ( 'NONE',  ( 17.95908333333332507, -2.390202921478481457, 8.894510420082752944 ) ) ;
#10768 = CARTESIAN_POINT ( 'NONE',  ( 2.835570222853222688, 11.82190223321585520, -3.905115993759757043 ) ) ;
#10769 = EDGE_CURVE ( 'NONE', #13583, #1109, #1333, .T. ) ;
#10770 = CARTESIAN_POINT ( 'NONE',  ( 24.08098870454836771, -2.879575660560934391, -8.995033484217190178 ) ) ;
#10771 = EDGE_CURVE ( 'NONE', #6636, #23948, #3059, .T. ) ;
#10772 = CARTESIAN_POINT ( 'NONE',  ( 1.677026364909826706, 30.52491814567345685, -1.541694782284209753 ) ) ;
#10773 = ORIENTED_EDGE ( 'NONE', *, *, #5719, .T. ) ;
#10774 = CARTESIAN_POINT ( 'NONE',  ( 1.536366799937312067, 24.28333333333333854, 1.999167105995431237 ) ) ;
#10775 = CARTESIAN_POINT ( 'NONE',  ( 2.000000000000000000, 30.00000000000000000, 3.464101615137999968 ) ) ;
#10776 = CIRCLE ( 'NONE', #6508, 0.1000000000000002554 ) ;
#10777 = CARTESIAN_POINT ( 'NONE',  ( 14.70937642131000089, 0.7886220128679000130, 9.636901145054999063 ) ) ;
#10778 = CARTESIAN_POINT ( 'NONE',  ( 18.45579459229852759, 9.947470068809831645, -3.106797963599987611 ) ) ;
#10779 = ORIENTED_EDGE ( 'NONE', *, *, #5925, .T. ) ;
#10780 = CARTESIAN_POINT ( 'NONE',  ( -1.536366799937282313, 29.15086340285666822, 1.999167105995454552 ) ) ;
#10781 = CARTESIAN_POINT ( 'NONE',  ( -0.3786279377524999767, 29.16623056986999885, -2.117165371715000077 ) ) ;
#10782 = CARTESIAN_POINT ( 'NONE',  ( 19.05150246751999887, -4.061773497662999333, 10.04047824780999854 ) ) ;
#10783 = CARTESIAN_POINT ( 'NONE',  ( 13.50000000000000000, -9.094337642950469203, 3.923034256449659640 ) ) ;
#10784 = ORIENTED_EDGE ( 'NONE', *, *, #9505, .F. ) ;
#10785 = CARTESIAN_POINT ( 'NONE',  ( -2.949999999999999734, 24.49999999999999645, 0.000000000000000000 ) ) ;
#10786 = CARTESIAN_POINT ( 'NONE',  ( -24.48376588670970833, -11.33649700729262300, 5.364757780054595138 ) ) ;
#10787 = VECTOR ( 'NONE', #11492, 1000.000000000000114 ) ;
#10788 = CARTESIAN_POINT ( 'NONE',  ( 1.999167105995462990, 29.11666666666667780, 1.536366799937272987 ) ) ;
#10789 = CARTESIAN_POINT ( 'NONE',  ( 0.000000000000000000, 30.00000000000000000, 0.000000000000000000 ) ) ;
#10790 = CARTESIAN_POINT ( 'NONE',  ( -4.155850825563766726, 13.71339692482677108, 4.894222041114647759 ) ) ;
#10791 = AXIS2_PLACEMENT_3D ( 'NONE', #1707, #7386, #18199 ) ;
#10792 = CARTESIAN_POINT ( 'NONE',  ( -3.747811089796003525, 12.10619433494998631, 3.242694335594999977 ) ) ;
#10793 = FACE_OUTER_BOUND ( 'NONE', #12445, .T. ) ;
#10794 = ORIENTED_EDGE ( 'NONE', *, *, #10459, .T. ) ;
#10795 = CARTESIAN_POINT ( 'NONE',  ( 23.41677564524290744, 35.51856778792605240, -6.000000000000000000 ) ) ;
#10796 = CARTESIAN_POINT ( 'NONE',  ( 1.762815800531199351, 13.00000000278783219, 1.071352341330493507 ) ) ;
#10797 = CONICAL_SURFACE ( 'NONE', #22003, 2.249999993254999886, 0.7853981633972997312 ) ;
#10798 = ORIENTED_EDGE ( 'NONE', *, *, #8358, .T. ) ;
#10799 = CARTESIAN_POINT ( 'NONE',  ( 0.6222432282865000275, 24.18601452002999608, 2.467948282817999939 ) ) ;
#10800 = DIRECTION ( 'NONE',  ( 0.000000000000000000, -1.000000000000000000, 0.000000000000000000 ) ) ;
#10801 = CARTESIAN_POINT ( 'NONE',  ( 11.22285964975960759, 2.000465806355621545, -12.49999014999358593 ) ) ;
#10802 = DIRECTION ( 'NONE',  ( -0.000000000000000000, 1.000000000000000000, -0.000000000000000000 ) ) ;
#10803 = DIRECTION ( 'NONE',  ( 0.000000000000000000, 1.000000000000000000, 0.000000000000000000 ) ) ;
#10804 = VECTOR ( 'NONE', #17573, 1000.000000000000000 ) ;
#10805 = CARTESIAN_POINT ( 'NONE',  ( 2.500000000000000000, 24.50000000000000000, 2.004655647840161273E-15 ) ) ;
#10806 = VERTEX_POINT ( 'NONE', #20840 ) ;
#10807 = DIRECTION ( 'NONE',  ( 0.000000000000000000, -1.000000000000000000, 0.000000000000000000 ) ) ;
#10808 = B_SPLINE_CURVE_WITH_KNOTS ( 'NONE', 3,
 ( #23217, #4712, #10641, #13897, #17662, #1189, #11234, #22009, #14499, #3957, #18370, #11349, #3496, #9405, #7574, #9291, #13030, #21891, #10876, #7108, #22230, #9052 ),
 .UNSPECIFIED., .F., .F.,
 ( 4, 2, 2, 2, 2, 2, 2, 2, 2, 2, 4 ),
 ( 3.041894376390393310E-05, 0.0007972261352801803414, 0.001564033326796456912, 0.002330840518312733266, 0.002714244114070871444, 0.002905945911949940966, 0.003001796810889475076, 0.003013778173256916569, 0.003025759535624358062, 0.003049722260359241047, 0.003097647709829007018 ),
 .UNSPECIFIED. ) ;
#10809 = CARTESIAN_POINT ( 'NONE',  ( -1.965891356465660378, 26.25632797282960951, 0.8861481259685903833 ) ) ;
#10810 = CARTESIAN_POINT ( 'NONE',  ( 30.87226923053214378, 27.01856778792605240, 2.673746900119611247 ) ) ;
#10811 = ORIENTED_EDGE ( 'NONE', *, *, #10087, .T. ) ;
#10812 = CLOSED_SHELL ( 'NONE', ( #16465, #18241, #5537, #5586, #8201, #11785, #20369, #9089, #11019, #15142, #21395, #7564, #718, #17256, #23641, #16340, #2984, #13564, #3526, #15894, #616, #19293, #21040, #2331, #2135, #12636, #7407, #14105, #21861, #10724, #6217, #6542, #365, #7445, #8675, #8078, #8319, #5258, #21105, #20772, #4050, #2285, #22583, #16653, #11796, #12064, #10900, #23696, #19852, #14217, #17824, #6151, #18268, #19426, #23726, #13787, #8494, #5559, #6356, #18701, #3785, #7758, #4250, #22700, #5359, #13192, #14128, #15715, #10754, #6690, #8809, #8554, #21383, #3753, #10292, #12681, #11187, #16792, #12415, #1303, #18096, #1124, #4382, #16740, #2602, #9533, #6274, #2434, #1077, #11662, #20938, #12926, #20418, #13320, #18837, #1302, #19444, #4060, #8366, #12045, #17468, #3949, #2845, #23174, #5100, #13949, #3181, #6589, #19867, #11632, #1381, #8039, #2777, #15017, #10023, #23292, #8898, #20815, #7471, #17387, #15547 ) ) ;
#10813 = CARTESIAN_POINT ( 'NONE',  ( -10.81061242803241207, 15.37188199527473209, -1.657872610222045129 ) ) ;
#10814 = CARTESIAN_POINT ( 'NONE',  ( 0.2479243946193999959, 24.70525031395999704, 2.130229948954000196 ) ) ;
#10815 = CARTESIAN_POINT ( 'NONE',  ( 14.81476371884029497, 9.716835099164804035, -3.542462622313707232 ) ) ;
#10816 = AXIS2_PLACEMENT_3D ( 'NONE', #19204, #6492, #13875 ) ;
#10817 = DIRECTION ( 'NONE',  ( 1.000000000000000000, 0.000000000000000000, 0.000000000000000000 ) ) ;
#10818 = CARTESIAN_POINT ( 'NONE',  ( 24.27251434224999826, -0.1538460603255000225, 11.30793493386000037 ) ) ;
#10819 = CARTESIAN_POINT ( 'NONE',  ( 1.596045994907000054, 30.58514805554999683, -1.467249313498999896 ) ) ;
#10820 = DIRECTION ( 'NONE',  ( -1.000000000000000000, 0.000000000000000000, 0.000000000000000000 ) ) ;
#10821 = CARTESIAN_POINT ( 'NONE',  ( -4.811303441321004293, 12.64225309966998623, 0.1541779168885000495 ) ) ;
#10822 = DIRECTION ( 'NONE',  ( 0.5882164119205371966, -0.8087035629619353516, 0.000000000000000000 ) ) ;
#10823 = AXIS2_PLACEMENT_3D ( 'NONE', #19963, #12696, #2022 ) ;
#10824 = ORIENTED_EDGE ( 'NONE', *, *, #12067, .T. ) ;
#10825 = CARTESIAN_POINT ( 'NONE',  ( -2.500000000000000000, 18.50000000000000000, 0.000000000000000000 ) ) ;
#10826 = CARTESIAN_POINT ( 'NONE',  ( -24.50000000000000000, -10.82531754731000007, -6.250000000000000000 ) ) ;
#10827 = CIRCLE ( 'NONE', #734, 1.000000000000000000 ) ;
#10828 = VECTOR ( 'NONE', #12716, 1000.000000000000000 ) ;
#10829 = VERTEX_POINT ( 'NONE', #13438 ) ;
#10830 = CARTESIAN_POINT ( 'NONE',  ( 11.39490977864411470, -12.26833003003723732, -3.750544030117427763 ) ) ;
#10831 = CARTESIAN_POINT ( 'NONE',  ( -6.000000000000000000, 24.99999999999999645, -6.000000000000000000 ) ) ;
#10832 = ADVANCED_BREP_SHAPE_REPRESENTATION ( '', ( #17244, #4390 ), #9795 ) ;
#10833 = CARTESIAN_POINT ( 'NONE',  ( 17.18559515836999907, -6.254670336401999542, 9.156935761679001473 ) ) ;
#10834 = ORIENTED_EDGE ( 'NONE', *, *, #15031, .F. ) ;
#10835 = CARTESIAN_POINT ( 'NONE',  ( -11.53092506584999910, 5.630713802624000230, 13.76055599481999892 ) ) ;
#10836 = FACE_OUTER_BOUND ( 'NONE', #5476, .T. ) ;
#10837 = CARTESIAN_POINT ( 'NONE',  ( -14.42499013958043541, -12.50426282925849897, -3.341925919231215403 ) ) ;
#10838 = AXIS2_PLACEMENT_3D ( 'NONE', #10249, #19704, #13998 ) ;
#10839 = EDGE_CURVE ( 'NONE', #20433, #16718, #5822, .T. ) ;
#10840 = EDGE_LOOP ( 'NONE', ( #728, #16230, #3860, #20006 ) ) ;
#10841 = CARTESIAN_POINT ( 'NONE',  ( 20.58796606631835857, 0.9461998122939191402, 10.48927542155332304 ) ) ;
#10842 = CARTESIAN_POINT ( 'NONE',  ( 12.50000000000000000, -13.93375672974000068, 0.000000000000000000 ) ) ;
#10843 = CARTESIAN_POINT ( 'NONE',  ( 16.01298929817072292, -8.180129550563604468, -6.355079070724960033 ) ) ;
#10844 = CARTESIAN_POINT ( 'NONE',  ( -1.499999883624000052, 7.099999883624000141, 4.580366260669000192E-07 ) ) ;
#10845 = CARTESIAN_POINT ( 'NONE',  ( 1.682158182759999843, 30.71240778275999972, -1.630908591657999951 ) ) ;
#10846 = AXIS2_PLACEMENT_3D ( 'NONE', #6379, #14139, #10147 ) ;
#10847 = CARTESIAN_POINT ( 'NONE',  ( -18.80493816619999947, -6.461643014194000223, 6.332623921217999552 ) ) ;
#10848 = ADVANCED_FACE ( 'NONE', ( #2182 ), #20958, .F. ) ;
#10849 = CARTESIAN_POINT ( 'NONE',  ( 2.101274614680348929, 29.83358767967074598, -0.5022599295738957581 ) ) ;
#10850 = ORIENTED_EDGE ( 'NONE', *, *, #19473, .T. ) ;
#10851 = CARTESIAN_POINT ( 'NONE',  ( 20.86671680498296766, -1.970433400296279780, 10.35129057732945412 ) ) ;
#10852 = DIRECTION ( 'NONE',  ( -5.739718509874449091E-40, -1.792960224733999962E-10, 1.000000000000000000 ) ) ;
#10853 = VERTEX_POINT ( 'NONE', #11641 ) ;
#10854 = CARTESIAN_POINT ( 'NONE',  ( -2.070272442071251717, 23.66806414737387243, 0.6316710083233486595 ) ) ;
#10855 = CARTESIAN_POINT ( 'NONE',  ( -14.25243324638999809, -6.216878364870000340, -12.50000000000000000 ) ) ;
#10856 = CARTESIAN_POINT ( 'NONE',  ( 0.3698661250554000635, 11.49512849500999323, -4.800726696805998728 ) ) ;
#10857 = VERTEX_POINT ( 'NONE', #7762 ) ;
#10858 = CARTESIAN_POINT ( 'NONE',  ( 2.100000000000000089, 29.69999999999999929, 0.000000000000000000 ) ) ;
#10859 = EDGE_LOOP ( 'NONE', ( #15973, #14056, #11929, #8712, #20174, #4502, #10784 ) ) ;
#10860 = CARTESIAN_POINT ( 'NONE',  ( -0.6543697108981787469, 28.40086340285666822, 2.434931691670795484 ) ) ;
#10861 = DIRECTION ( 'NONE',  ( 0.000000000000000000, 1.000000000000000000, 0.000000000000000000 ) ) ;
#10862 = EDGE_CURVE ( 'NONE', #4095, #4052, #11520, .T. ) ;
#10863 = EDGE_LOOP ( 'NONE', ( #10419, #281, #2793, #20002 ) ) ;
#10864 = CARTESIAN_POINT ( 'NONE',  ( -15.30809587121333415, -4.564978959981946360, 7.920054021321541349 ) ) ;
#10865 = CARTESIAN_POINT ( 'NONE',  ( -21.22497918939999906, 2.624718450046000129, -9.764018522075000206 ) ) ;
#10866 = CARTESIAN_POINT ( 'NONE',  ( -19.41764062158999948, 9.069691137161999706, -3.822207856851999708 ) ) ;
#10867 = CARTESIAN_POINT ( 'NONE',  ( 6.696152422707000618, 28.00000000000000000, -6.000000000000000000 ) ) ;
#10868 = CARTESIAN_POINT ( 'NONE',  ( -23.16076897183521766, -10.23206097900809475, 2.674434693994577561 ) ) ;
#10869 = CARTESIAN_POINT ( 'NONE',  ( 1.625795695728253776, 26.51215493189252115, 1.441208665152567292 ) ) ;
#10870 = CARTESIAN_POINT ( 'NONE',  ( -2.505154520421000175, 28.92500240009999857, 1.402946323589000066 ) ) ;
#10871 = ADVANCED_FACE ( 'NONE', ( #20715 ), #23550, .T. ) ;
#10872 = CARTESIAN_POINT ( 'NONE',  ( -0.2434897306343792311, 30.81781537185297992, -2.179389815440565314 ) ) ;
#10873 = ORIENTED_EDGE ( 'NONE', *, *, #22973, .F. ) ;
#10874 = CARTESIAN_POINT ( 'NONE',  ( -1.099193499486128101, 26.43562577624027199, -3.984182490697167900 ) ) ;
#10875 = DIRECTION ( 'NONE',  ( 1.000000000000000000, 0.000000000000000000, 0.000000000000000000 ) ) ;
#10876 = CARTESIAN_POINT ( 'NONE',  ( 1.667713432661086959, 24.74980862569434237, 1.357244015048324925 ) ) ;
#10877 = CARTESIAN_POINT ( 'NONE',  ( -2.281391790424999844, 27.57614211382000136, -0.2246974795678000070 ) ) ;
#10878 = CIRCLE ( 'NONE', #23636, 12.44999999999999929 ) ;
#10879 = DIRECTION ( 'NONE',  ( 0.000000000000000000, 0.9999453485888588622, 0.01045465616390955921 ) ) ;
#10880 = ORIENTED_EDGE ( 'NONE', *, *, #15777, .T. ) ;
#10881 = EDGE_CURVE ( 'NONE', #5259, #16694, #4497, .T. ) ;
#10882 = CARTESIAN_POINT ( 'NONE',  ( -2.920465629076966163, 11.84211311063798888, -3.843655616409710873 ) ) ;
#10883 = CARTESIAN_POINT ( 'NONE',  ( 24.16322961496833344, 1.753000555242941516, -9.398851739486781653 ) ) ;
#10884 = FACE_OUTER_BOUND ( 'NONE', #13253, .T. ) ;
#10885 = EDGE_LOOP ( 'NONE', ( #1280, #21952, #11657, #2610 ) ) ;
#10886 = EDGE_CURVE ( 'NONE', #11418, #19500, #3407, .T. ) ;
#10887 = EDGE_CURVE ( 'NONE', #12189, #19402, #18888, .T. ) ;
#10888 = DIRECTION ( 'NONE',  ( 0.000000000000000000, 0.9999173538268769645, -0.01285634146465969990 ) ) ;
#10889 = LINE ( 'NONE', #12703, #311 ) ;
#10890 = CARTESIAN_POINT ( 'NONE',  ( 18.79425158531000051, -6.072333155528000681, 7.996935486658999892 ) ) ;
#10891 = CARTESIAN_POINT ( 'NONE',  ( 18.59376286737137818, 10.28297712058548008, 1.725429498650708160 ) ) ;
#10892 = UNCERTAINTY_MEASURE_WITH_UNIT (LENGTH_MEASURE( 1.000000000000000082E-05 ), #22052, 'distance_accuracy_value', 'NONE');
#10893 = DIRECTION ( 'NONE',  ( 0.000000000000000000, -1.000000000000000000, 0.000000000000000000 ) ) ;
#10894 = CARTESIAN_POINT ( 'NONE',  ( 1.696015419756000009, 29.82802777462000066, -1.322603481717999907 ) ) ;
#10895 = CARTESIAN_POINT ( 'NONE',  ( -12.49507687580999971, 6.705241787176000834, -5.996946098961000615 ) ) ;
#10896 = LINE ( 'NONE', #5096, #8532 ) ;
#10897 = ORIENTED_EDGE ( 'NONE', *, *, #2028, .T. ) ;
#10898 = CARTESIAN_POINT ( 'NONE',  ( 61.60588651278290939, 37.01856778792605240, 1.000000000000000000 ) ) ;
#10899 = CARTESIAN_POINT ( 'NONE',  ( 21.00984673308000339, -8.695248534891000247, 7.185696252475000101 ) ) ;
#10900 = ADVANCED_FACE ( 'NONE', ( #8967 ), #15402, .F. ) ;
#10901 = CARTESIAN_POINT ( 'NONE',  ( 0.000000000000000000, 13.10000000000000142, -4.724999999995985966 ) ) ;
#10902 = B_SPLINE_CURVE_WITH_KNOTS ( 'NONE', 3,
 ( #5358, #5704, #7880, #17079, #18901 ),
 .UNSPECIFIED., .F., .F.,
 ( 4, 1, 4 ),
 ( 0.000000000000000000, 0.5000000000000000000, 1.000000000000000000 ),
 .UNSPECIFIED. ) ;
#10903 = EDGE_CURVE ( 'NONE', #19902, #19018, #12016, .T. ) ;
#10904 = DIRECTION ( 'NONE',  ( 0.000000000000000000, 0.000000000000000000, 1.000000000000000000 ) ) ;
#10905 = FACE_OUTER_BOUND ( 'NONE', #21176, .T. ) ;
#10906 = CARTESIAN_POINT ( 'NONE',  ( -4.940722032108995521, 12.51282703623000536, -0.1567078306562000589 ) ) ;
#10907 = CARTESIAN_POINT ( 'NONE',  ( -1.240246564627624171, 29.28173428028883407, -1.768320821386759834 ) ) ;
#10908 = CARTESIAN_POINT ( 'NONE',  ( -24.14868686146999721, -0.7737383780821999180, -11.13665872500999932 ) ) ;
#10909 = VERTEX_POINT ( 'NONE', #22038 ) ;
#10910 = CARTESIAN_POINT ( 'NONE',  ( 1.702244497849941807, 12.92465160051537332, 1.054166248807005157 ) ) ;
#10911 = ORIENTED_EDGE ( 'NONE', *, *, #3708, .T. ) ;
#10912 = CARTESIAN_POINT ( 'NONE',  ( 5.805205508519002855, 13.82243867059999509, 2.388040532770999480 ) ) ;
#10913 = CARTESIAN_POINT ( 'NONE',  ( 11.48696334737532432, 3.271224437879761027, -12.49992143329918903 ) ) ;
#10914 = DIRECTION ( 'NONE',  ( 1.000000000000000000, -0.000000000000000000, -0.000000000000000000 ) ) ;
#10915 = CARTESIAN_POINT ( 'NONE',  ( 13.50000000000000178, -0.9241557808115162809, 10.25573529546197804 ) ) ;
#10916 = CIRCLE ( 'NONE', #23276, 2.999999999999999112 ) ;
#10917 = B_SPLINE_CURVE_WITH_KNOTS ( 'NONE', 3,
 ( #13078, #5693, #15234, #11630, #351, #17066, #16825, #20587, #18763, #16705, #18654, #20705, #9801, #11511, #2060, #2174, #13551, #7628, #5812, #463, #2411, #15005, #581, #7867, #22404, #13195, #7986, #15116, #3997, #9566, #2297, #22514 ),
 .UNSPECIFIED., .F., .F.,
 ( 4, 2, 2, 2, 2, 2, 2, 2, 2, 2, 2, 2, 2, 2, 2, 4 ),
 ( 0.000000000000000000, 0.1250000000000000555, 0.1875000000000001943, 0.2187500000000002220, 0.2500000000000002220, 0.3125000000000002220, 0.3437500000000002220, 0.3750000000000002220, 0.5000000000000003331, 0.5625000000000003331, 0.5937500000000003331, 0.6250000000000004441, 0.6875000000000004441, 0.7187500000000004441, 0.7500000000000004441, 1.000000000000000000 ),
 .UNSPECIFIED. ) ;
#10918 = ORIENTED_EDGE ( 'NONE', *, *, #10142, .F. ) ;
#10919 = CARTESIAN_POINT ( 'NONE',  ( -17.99241677431999875, 4.425129475628999387, -8.746809379632999537 ) ) ;
#10920 = DIRECTION ( 'NONE',  ( 0.000000000000000000, 1.000000000000000000, 0.000000000000000000 ) ) ;
#10921 = CARTESIAN_POINT ( 'NONE',  ( 0.000000000000000000, 22.00000000000000000, 0.000000000000000000 ) ) ;
#10922 = ORIENTED_EDGE ( 'NONE', *, *, #6971, .F. ) ;
#10923 = DIRECTION ( 'NONE',  ( 0.000000000000000000, -1.000000000000000000, 0.000000000000000000 ) ) ;
#10924 = CARTESIAN_POINT ( 'NONE',  ( -2.329416328254999780, 25.17618571299000152, -0.1626863643163999895 ) ) ;
#10925 = CARTESIAN_POINT ( 'NONE',  ( 14.72221008384615182, 8.065344004061731908, -6.473147478577542024 ) ) ;
#10926 = CIRCLE ( 'NONE', #14011, 7.000000000000000000 ) ;
#10927 = CARTESIAN_POINT ( 'NONE',  ( -18.55817920454666847, -8.909387095795679556, -2.394461597111133155 ) ) ;
#10928 = CARTESIAN_POINT ( 'NONE',  ( 19.13319937917999880, -9.753461774593999323, 5.439862873842999491 ) ) ;
#10929 = CARTESIAN_POINT ( 'NONE',  ( 2.112897800473000132, 28.86173480117000167, 0.4856074845446999855 ) ) ;
#10930 = CARTESIAN_POINT ( 'NONE',  ( 14.04262667236427831, 6.000419062831993777, 6.762735978225977718 ) ) ;
#10931 = CARTESIAN_POINT ( 'NONE',  ( 4.795731778619003904, 12.63621800153999075, -0.5225435171593996175 ) ) ;
#10932 = SURFACE_STYLE_FILL_AREA ( #3548 ) ;
#10933 = ORIENTED_EDGE ( 'NONE', *, *, #7433, .F. ) ;
#10934 = CARTESIAN_POINT ( 'NONE',  ( -14.86522788937946338, -8.015611292679002631, -4.223672244188741765 ) ) ;
#10935 = AXIS2_PLACEMENT_3D ( 'NONE', #4272, #20975, #8512 ) ;
#10936 = DIRECTION ( 'NONE',  ( -1.000000000000000000, 0.000000000000000000, 0.000000000000000000 ) ) ;
#10937 = ORIENTED_EDGE ( 'NONE', *, *, #5722, .T. ) ;
#10938 = CARTESIAN_POINT ( 'NONE',  ( -15.61632910584000022, 9.072027496059000384, 0.000000000000000000 ) ) ;
#10939 = CARTESIAN_POINT ( 'NONE',  ( 11.48478210364763541, -12.46109695279135288, -3.416571976975812941 ) ) ;
#10940 = DIRECTION ( 'NONE',  ( 0.9996708941621513800, -0.02565352539213145919, 0.000000000000000000 ) ) ;
#10941 = CARTESIAN_POINT ( 'NONE',  ( 15.05401368519000016, -0.07836042960794999124, 11.03054286538000106 ) ) ;
#10942 = CARTESIAN_POINT ( 'NONE',  ( -14.11172255407341325, -5.446421583873537031, 8.794184178919268291 ) ) ;
#10943 = ORIENTED_EDGE ( 'NONE', *, *, #1977, .F. ) ;
#10944 = CARTESIAN_POINT ( 'NONE',  ( -10.09803613877000039, -2.313608892657999849, 15.04153609805999992 ) ) ;
#10945 = CARTESIAN_POINT ( 'NONE',  ( 13.50000000000000000, 7.641056615018084308, -5.228549223296183435 ) ) ;
#10946 = DIRECTION ( 'NONE',  ( 0.000000000000000000, 0.000000000000000000, 1.000000000000000000 ) ) ;
#10947 = ORIENTED_EDGE ( 'NONE', *, *, #4698, .F. ) ;
#10948 = CARTESIAN_POINT ( 'NONE',  ( 23.11762048267087977, -7.246916755350970796, -7.729893100918809878 ) ) ;
#10949 = CONICAL_SURFACE ( 'NONE', #23702, 3.049999825846000157, 0.7853981633972997312 ) ;
#10950 = CARTESIAN_POINT ( 'NONE',  ( 4.649999849441000421, 17.00000015055400127, -6.648422772555000414E-08 ) ) ;
#10951 = CARTESIAN_POINT ( 'NONE',  ( 16.18882540054575259, -3.105308896812054797, -9.887464255232517374 ) ) ;
#10952 = CARTESIAN_POINT ( 'NONE',  ( -4.982685754363140873, 13.67876053192405905, 5.582247605641564192 ) ) ;
#10953 = CARTESIAN_POINT ( 'NONE',  ( -14.39391672138606992, -12.88860090843611061, 2.676267392864990491 ) ) ;
#10954 = DIRECTION ( 'NONE',  ( 1.000000000000000000, 4.862776847858214598E-10, 0.000000000000000000 ) ) ;
#10955 = CARTESIAN_POINT ( 'NONE',  ( 1.712616862212509972, 29.88731553013089126, -1.316065052317139772 ) ) ;
#10956 = EDGE_LOOP ( 'NONE', ( #117, #23371, #15928 ) ) ;
#10957 = CARTESIAN_POINT ( 'NONE',  ( -0.5315530086984000535, 23.66540885998999855, -2.041217608508999692 ) ) ;
#10958 = CARTESIAN_POINT ( 'NONE',  ( 19.67503469114785730, -7.524009671958713952, -7.334830238956850934 ) ) ;
#10959 = CARTESIAN_POINT ( 'NONE',  ( 1.709999999999999964, 9.852710287022999225, 7.500000000000000000 ) ) ;
#10960 = VERTEX_POINT ( 'NONE', #9195 ) ;
#10961 = EDGE_CURVE ( 'NONE', #14047, #2380, #11172, .T. ) ;
#10962 = DIRECTION ( 'NONE',  ( 0.000000000000000000, 1.000000000000000000, 0.000000000000000000 ) ) ;
#10963 = DIRECTION ( 'NONE',  ( -1.000000000000000000, 0.000000000000000000, 0.000000000000000000 ) ) ;
#10964 = AXIS2_PLACEMENT_3D ( 'NONE', #13303, #17406, #2872 ) ;
#10965 = CARTESIAN_POINT ( 'NONE',  ( -3.196386508574998953, 11.94625779823998357, -3.568797075887999437 ) ) ;
#10966 = VERTEX_POINT ( 'NONE', #19986 ) ;
#10967 = CARTESIAN_POINT ( 'NONE',  ( 16.35468892131000018, 6.000265896171000257, 7.637201470843999473 ) ) ;
#10968 = ORIENTED_EDGE ( 'NONE', *, *, #11634, .T. ) ;
#10969 = CARTESIAN_POINT ( 'NONE',  ( -5.050080520837401110, 15.90270261739640922, 3.465883707748838916 ) ) ;
#10970 = VECTOR ( 'NONE', #23775, 1000.000000000000114 ) ;
#10971 = ITEM_DEFINED_TRANSFORMATION ( 'NONE', 'NONE', #10187,  #4390 ) ;
#10972 = CARTESIAN_POINT ( 'NONE',  ( -2.102266727616999731, 23.66000000000000014, 0.4960590750638999569 ) ) ;
#10973 = EDGE_CURVE ( 'NONE', #17884, #20779, #7673, .T. ) ;
#10974 = ORIENTED_EDGE ( 'NONE', *, *, #3651, .F. ) ;
#10975 = CARTESIAN_POINT ( 'NONE',  ( -15.87497087121333017, 9.078664753515003127, 1.188521384907375467 ) ) ;
#10976 = CARTESIAN_POINT ( 'NONE',  ( -19.99381460464000071, -9.570925607007000124, 1.774722651697000053 ) ) ;
#10977 = DIRECTION ( 'NONE',  ( 1.000000000000000000, 0.000000000000000000, 0.000000000000000000 ) ) ;
#10978 = CARTESIAN_POINT ( 'NONE',  ( -5.542211513735998629, 15.02033096712999338, -2.995715936518001499 ) ) ;
#10979 = CARTESIAN_POINT ( 'NONE',  ( -22.13136394192933665, 10.52421200172316951, 1.769957956558704026 ) ) ;
#10980 = CARTESIAN_POINT ( 'NONE',  ( -0.7372999604405595653, 27.16143315320393015, 2.077662471664349475 ) ) ;
#10981 = CARTESIAN_POINT ( 'NONE',  ( -12.25000000000000000, 1.374666032043000015E-14, 0.000000000000000000 ) ) ;
#10982 = CARTESIAN_POINT ( 'NONE',  ( 1.838512823634357529, 30.67449951250407381, -1.138862448013022277 ) ) ;
#10983 = VERTEX_POINT ( 'NONE', #23618 ) ;
#10984 = CARTESIAN_POINT ( 'NONE',  ( 4.787200832998987465, 14.77986595429568162, 3.821410012779939969 ) ) ;
#10985 = CARTESIAN_POINT ( 'NONE',  ( 14.46456608149148515, 2.351140429448762337, 8.785231713726679104 ) ) ;
#10986 = B_SPLINE_CURVE_WITH_KNOTS ( 'NONE', 3,
 ( #11223, #4062, #13145, #19066, #15429, #13258, #9630, #17015, #3827, #173, #13370, #5873, #20773, #4179, #11456, #8057, #20538, #15302 ),
 .UNSPECIFIED., .F., .F.,
 ( 4, 2, 2, 2, 2, 2, 2, 2, 4 ),
 ( 0.000000000000000000, 0.1250000000000000000, 0.2500000000000000555, 0.3750000000000001110, 0.5000000000000001110, 0.6250000000000001110, 0.7500000000000001110, 0.8750000000000001110, 1.000000000000000000 ),
 .UNSPECIFIED. ) ;
#10987 = EDGE_CURVE ( 'NONE', #14560, #4269, #11131, .T. ) ;
#10988 = CARTESIAN_POINT ( 'NONE',  ( 1.196956196243999848, 25.94937716036000097, -2.137330684255000168 ) ) ;
#10989 = CYLINDRICAL_SURFACE ( 'NONE', #5012, 1.500000000000000000 ) ;
#10990 = CARTESIAN_POINT ( 'NONE',  ( 0.8369952473213599919, 11.51240063293612970, 4.739979841301923180 ) ) ;
#10991 = ORIENTED_EDGE ( 'NONE', *, *, #17688, .T. ) ;
#10992 = CARTESIAN_POINT ( 'NONE',  ( -1.122479358643900360, 11.53522643002050074, -4.684283708769314991 ) ) ;
#10993 = CARTESIAN_POINT ( 'NONE',  ( -10.65331237176230950, 15.43888331649234225, 1.511769160805160217 ) ) ;
#10994 = CARTESIAN_POINT ( 'NONE',  ( 0.2381761436251323971, 29.01693154808815223, -2.265505022230542398 ) ) ;
#10995 = ORIENTED_EDGE ( 'NONE', *, *, #2527, .F. ) ;
#10996 = EDGE_CURVE ( 'NONE', #6063, #10960, #14268, .T. ) ;
#10997 = CARTESIAN_POINT ( 'NONE',  ( 4.000000000000000000, 24.50000000000000000, -2.309401076759000304 ) ) ;
#10998 = CARTESIAN_POINT ( 'NONE',  ( 60.61494135913342518, 27.01856778792605240, 0.000000000000000000 ) ) ;
#10999 = CARTESIAN_POINT ( 'NONE',  ( 14.84550158531000008, 4.534570621724000716, 9.116298118718001220 ) ) ;
#11000 = CARTESIAN_POINT ( 'NONE',  ( 18.61878911107620382, 10.09093427090647666, 2.640026560685321044 ) ) ;
#11001 = CARTESIAN_POINT ( 'NONE',  ( -2.500000000000000444, 29.05086340285667035, 0.3272492347489422415 ) ) ;
#11002 = CARTESIAN_POINT ( 'NONE',  ( 2.128941206161000466, 29.76184805414000323, -0.3055447833205000019 ) ) ;
#11003 = AXIS2_PLACEMENT_3D ( 'NONE', #23170, #10353, #17741 ) ;
#11004 = DIRECTION ( 'NONE',  ( 1.000000000000000000, 0.000000000000000000, 0.000000000000000000 ) ) ;
#11005 = CARTESIAN_POINT ( 'NONE',  ( 13.49999999999999645, -9.561895257915249857, -0.9817478549585191283 ) ) ;
#11006 = EDGE_LOOP ( 'NONE', ( #9320, #21851, #5059, #21148 ) ) ;
#11007 = ADVANCED_FACE ( 'NONE', ( #7483 ), #18182, .F. ) ;
#11008 = PLANE ( 'NONE',  #3682 ) ;
#11009 = CARTESIAN_POINT ( 'NONE',  ( 23.58278963329000177, -5.861239335239000425, -9.096485928357999740 ) ) ;
#11010 = CARTESIAN_POINT ( 'NONE',  ( 2.184465970885653530, 29.13333333333333997, 1.259047450927233802 ) ) ;
#11011 = CARTESIAN_POINT ( 'NONE',  ( 4.000000000000000000, 24.80000000000000426, 2.309401076759000304 ) ) ;
#11012 = CARTESIAN_POINT ( 'NONE',  ( -5.730762473771000565, 26.50000000000000000, 1.577381738259000077 ) ) ;
#11013 = AXIS2_PLACEMENT_3D ( 'NONE', #12376, #14304, #7029 ) ;
#11014 = CARTESIAN_POINT ( 'NONE',  ( -4.899115602372003941, 12.43333805657998603, 0.4236866773311000478 ) ) ;
#11015 = CARTESIAN_POINT ( 'NONE',  ( -1.402904250052608104, 29.29391569701615694, -1.642719484273872377 ) ) ;
#11016 = ADVANCED_FACE ( 'NONE', ( #16449, #5330 ), #8856, .T. ) ;
#11017 = CARTESIAN_POINT ( 'NONE',  ( -12.24999999999999822, 13.59206128970241778, -6.344557540553090291 ) ) ;
#11018 = VERTEX_POINT ( 'NONE', #692 ) ;
#11019 = ADVANCED_FACE ( 'NONE', ( #15216 ), #11937, .T. ) ;
#11020 = CARTESIAN_POINT ( 'NONE',  ( 66.60588651278291650, 35.51856778792605240, -1.000000000000000000 ) ) ;
#11021 = EDGE_LOOP ( 'NONE', ( #17030, #16528, #20835, #716 ) ) ;
#11022 = CARTESIAN_POINT ( 'NONE',  ( 1.189766245367999797, 24.91662324376000015, 2.030297963902000014 ) ) ;
#11023 = CARTESIAN_POINT ( 'NONE',  ( 5.182093470520005241, 14.34449281741999727, 3.190697958076003093 ) ) ;
#11024 = CARTESIAN_POINT ( 'NONE',  ( 6.696152422707000618, 28.00000000000000000, 6.000000000000000000 ) ) ;
#11025 = B_SPLINE_CURVE_WITH_KNOTS ( 'NONE', 3,
 ( #9024, #21748, #5161, #15913, #16280, #18119, #8914, #14469, #19573, #12305, #12661, #21384, #4799, #4919 ),
 .UNSPECIFIED., .F., .F.,
 ( 4, 2, 2, 2, 2, 2, 4 ),
 ( 0.000000000000000000, 0.2500000000000007772, 0.3750000000000008327, 0.5000000000000006661, 0.6250000000000004441, 0.7500000000000003331, 1.000000000000000000 ),
 .UNSPECIFIED. ) ;
#11026 = CARTESIAN_POINT ( 'NONE',  ( 18.98579496512684628, -1.886667643284684948, 10.26048715248877485 ) ) ;
#11027 = DIRECTION ( 'NONE',  ( -1.000000000000000000, 0.000000000000000000, 0.000000000000000000 ) ) ;
#11028 = CARTESIAN_POINT ( 'NONE',  ( 11.81081408531000143, -9.938255359128000066, -0.2191561108886999898 ) ) ;
#11029 = EDGE_CURVE ( 'NONE', #7614, #18970, #21625, .T. ) ;
#11030 = ORIENTED_EDGE ( 'NONE', *, *, #8309, .T. ) ;
#11031 = CARTESIAN_POINT ( 'NONE',  ( 2.729128784747790970, 18.00000000000000000, 0.000000000000000000 ) ) ;
#11032 = AXIS2_PLACEMENT_3D ( 'NONE', #16088, #14294, #10426 ) ;
#11033 = B_SPLINE_CURVE_WITH_KNOTS ( 'NONE', 3,
 ( #2728, #19441, #13492, #2477 ),
 .UNSPECIFIED., .F., .F.,
 ( 4, 4 ),
 ( 0.000000000000000000, 1.000000000000000000 ),
 .UNSPECIFIED. ) ;
#11034 = CARTESIAN_POINT ( 'NONE',  ( 14.99328936713000004, -9.056039068417000237, 0.000000000000000000 ) ) ;
#11035 = CARTESIAN_POINT ( 'NONE',  ( 23.15628936713000030, 9.265517736846000219, 0.000000000000000000 ) ) ;
#11036 = ORIENTED_EDGE ( 'NONE', *, *, #14325, .F. ) ;
#11037 = CARTESIAN_POINT ( 'NONE',  ( -22.56211168660000155, -2.887064115966999633, -10.88924876608999881 ) ) ;
#11038 = CARTESIAN_POINT ( 'NONE',  ( -2.119341350454000406, 25.24022682738999990, 0.9803262384023999632 ) ) ;
#11039 = CARTESIAN_POINT ( 'NONE',  ( 14.69340912245870001, 7.378059427811160198, -7.245375437766548465 ) ) ;
#11040 = FACE_OUTER_BOUND ( 'NONE', #7042, .T. ) ;
#11041 = CARTESIAN_POINT ( 'NONE',  ( 23.09738183229000086, -10.55345434226000023, 3.972832674855999890 ) ) ;
#11042 = CARTESIAN_POINT ( 'NONE',  ( 2.021323174276000056, 30.26884416382999987, -1.858207751705999833 ) ) ;
#11043 = CARTESIAN_POINT ( 'NONE',  ( 13.93170734267679123, 8.120445290024731477, 4.030814257595042527 ) ) ;
#11044 = CARTESIAN_POINT ( 'NONE',  ( -6.461264013247827620, 15.49809339140494480, -1.417960285014638444 ) ) ;
#11045 = CARTESIAN_POINT ( 'NONE',  ( 0.000000000000000000, 29.85000000000000142, 0.000000000000000000 ) ) ;
#11046 = ADVANCED_FACE ( 'NONE', ( #2393 ), #13645, .F. ) ;
#11047 = ORIENTED_EDGE ( 'NONE', *, *, #20329, .T. ) ;
#11048 = EDGE_CURVE ( 'NONE', #22927, #14207, #446, .T. ) ;
#11049 = AXIS2_PLACEMENT_3D ( 'NONE', #8093, #6380, #13284 ) ;
#11050 = CARTESIAN_POINT ( 'NONE',  ( 24.50000000000000355, -9.703066433905631172, -2.676520811178526582 ) ) ;
#11051 = ORIENTED_EDGE ( 'NONE', *, *, #4509, .F. ) ;
#11052 = CARTESIAN_POINT ( 'NONE',  ( -16.10762077250664248, -1.189048994148048655, -9.084635008511355636 ) ) ;
#11053 = DIRECTION ( 'NONE',  ( 1.000000000000000000, 0.000000000000000000, 0.000000000000000000 ) ) ;
#11054 = CARTESIAN_POINT ( 'NONE',  ( 6.696152422707000618, 29.50000000000000000, -6.000000000000000000 ) ) ;
#11055 = CARTESIAN_POINT ( 'NONE',  ( 14.62545328758000096, 6.656066219229999525, -8.781628413182000159 ) ) ;
#11056 = DIRECTION ( 'NONE',  ( -1.000000000000000000, -0.000000000000000000, -0.000000000000000000 ) ) ;
#11057 = CARTESIAN_POINT ( 'NONE',  ( -0.2616786785208999877, 26.49212896666999839, -2.656868203660999850 ) ) ;
#11058 = EDGE_CURVE ( 'NONE', #8671, #4782, #13408, .T. ) ;
#11059 = ORIENTED_EDGE ( 'NONE', *, *, #22244, .F. ) ;
#11060 = EDGE_CURVE ( 'NONE', #20057, #19401, #11954, .T. ) ;
#11061 = CARTESIAN_POINT ( 'NONE',  ( -10.50532613877000010, 15.21613563232000033, 0.2642172441792000614 ) ) ;
#11062 = DIRECTION ( 'NONE',  ( 1.000000000000000000, 0.000000000000000000, 9.309572557292015679E-11 ) ) ;
#11063 = CARTESIAN_POINT ( 'NONE',  ( -14.00000000000000000, 1.396097351027999937E-14, 0.000000000000000000 ) ) ;
#11064 = CIRCLE ( 'NONE', #5262, 9.974367097859005327 ) ;
#11065 = VERTEX_POINT ( 'NONE', #20687 ) ;
#11066 = CARTESIAN_POINT ( 'NONE',  ( -6.250000000000000000, -15.43375672974000068, 0.000000000000000000 ) ) ;
#11067 = CARTESIAN_POINT ( 'NONE',  ( 20.51087270046332733, -8.958289992760562370, -2.407343205403928099 ) ) ;
#11068 = VECTOR ( 'NONE', #2582, 1000.000000000000000 ) ;
#11069 = CARTESIAN_POINT ( 'NONE',  ( 23.99062354302999722, 7.716878364870000340, -11.63397459621999985 ) ) ;
#11070 = CARTESIAN_POINT ( 'NONE',  ( 16.02151485735762293, -7.988024155100645451, -6.595574518746330384 ) ) ;
#11071 = CARTESIAN_POINT ( 'NONE',  ( -13.62914419562999946, -10.20270304202000133, -2.517845328698999907 ) ) ;
#11072 = CARTESIAN_POINT ( 'NONE',  ( -0.9067637935996000209, 30.06497459668999994, -2.160393313164000073 ) ) ;
#11073 = CARTESIAN_POINT ( 'NONE',  ( -4.000000000000073719, 28.20197603011089527, -1.905018119001588683 ) ) ;
#11074 = CARTESIAN_POINT ( 'NONE',  ( 0.7476305753117580277, 29.95889564184829368, -2.026589009648734674 ) ) ;
#11075 = VERTEX_POINT ( 'NONE', #22851 ) ;
#11076 = CARTESIAN_POINT ( 'NONE',  ( -1.344757420832000117, 25.31728931014000139, -1.717707233910999998 ) ) ;
#11077 = CARTESIAN_POINT ( 'NONE',  ( 19.95876852777634625, 1.938386817457601108, -10.33238417878841631 ) ) ;
#11078 = CARTESIAN_POINT ( 'NONE',  ( -5.833999999999999631, -12.89775331292639926, -5.076083135505105348E-10 ) ) ;
#11079 = EDGE_LOOP ( 'NONE', ( #14938, #8142, #16187, #19560, #18680 ) ) ;
#11080 = CARTESIAN_POINT ( 'NONE',  ( 5.302309868036999774, 13.73032359673999814, 4.450989051274000019 ) ) ;
#11081 = AXIS2_PLACEMENT_3D ( 'NONE', #17546, #942, #8707 ) ;
#11082 = AXIS2_PLACEMENT_3D ( 'NONE', #3160, #4607, #12117 ) ;
#11083 = CARTESIAN_POINT ( 'NONE',  ( 4.818401220988001832, 12.41582519560999032, -0.5157391765471998069 ) ) ;
#11084 = CARTESIAN_POINT ( 'NONE',  ( 15.45075125730999943, 1.788522226178000052, -9.003565944673999510 ) ) ;
#11085 = EDGE_LOOP ( 'NONE', ( #10873, #13668, #15349, #6565 ) ) ;
#11086 = DIRECTION ( 'NONE',  ( 1.561251128379125123E-14, -1.000000000000000000, 0.000000000000000000 ) ) ;
#11087 = B_SPLINE_CURVE_WITH_KNOTS ( 'NONE', 3,
 ( #11980, #22858, #6272, #21302 ),
 .UNSPECIFIED., .F., .F.,
 ( 4, 4 ),
 ( 0.000000000000000000, 1.000000000000000000 ),
 .UNSPECIFIED. ) ;
#11088 = APPLICATION_PROTOCOL_DEFINITION ( 'draft international standard', 'automotive_design', 1998, #17953 ) ;
#11089 = DIRECTION ( 'NONE',  ( 0.000000000000000000, -1.000000000000000000, 0.000000000000000000 ) ) ;
#11090 = VERTEX_POINT ( 'NONE', #7969 ) ;
#11091 = AXIS2_PLACEMENT_3D ( 'NONE', #22820, #6235, #7701 ) ;
#11092 = CARTESIAN_POINT ( 'NONE',  ( -17.72676253787999912, 9.126185377371999863, 0.000000000000000000 ) ) ;
#11093 = CARTESIAN_POINT ( 'NONE',  ( 12.00000000000000178, 1.904880462199602054, -9.045477544701622463 ) ) ;
#11094 = EDGE_CURVE ( 'NONE', #19490, #9699, #11727, .T. ) ;
#11095 = CARTESIAN_POINT ( 'NONE',  ( 0.000000000000000000, 12.37689379448999993, 0.000000000000000000 ) ) ;
#11096 = DIRECTION ( 'NONE',  ( 0.000000000000000000, 0.000000000000000000, 1.000000000000000000 ) ) ;
#11097 = CARTESIAN_POINT ( 'NONE',  ( -21.92548293594716924, 6.766409901490216150, 8.245667780346659370 ) ) ;
#11098 = CARTESIAN_POINT ( 'NONE',  ( -1.888459278277104156E-11, 26.49469377355791977, -2.394693773557865057 ) ) ;
#11099 = CIRCLE ( 'NONE', #14948, 7.500000000000000000 ) ;
#11100 = CARTESIAN_POINT ( 'NONE',  ( 6.117240279542961012, 14.37689077026887041, 0.3699855186153612197 ) ) ;
#11101 = CARTESIAN_POINT ( 'NONE',  ( -4.649999849441000421, 22.00000015055399771, 6.648422636708999828E-08 ) ) ;
#11102 = CARTESIAN_POINT ( 'NONE',  ( 1.247171621864741953, 30.72546509146406279, -1.763763891515052640 ) ) ;
#11103 = ORIENTED_EDGE ( 'NONE', *, *, #14565, .F. ) ;
#11104 = CARTESIAN_POINT ( 'NONE',  ( 2.210755315046764480, 26.34981806843837759, 0.4830521748348369782 ) ) ;
#11105 = CARTESIAN_POINT ( 'NONE',  ( 4.369209802590991565, 13.43978707160767883, -5.263635815137498675 ) ) ;
#11106 = CARTESIAN_POINT ( 'NONE',  ( -24.12520316825921896, 4.399791340197258371, -9.646299765070683208 ) ) ;
#11107 = CARTESIAN_POINT ( 'NONE',  ( -2.392615059649000120, 26.24187716036000495, 0.5249584007626999504 ) ) ;
#11108 = DIRECTION ( 'NONE',  ( 1.000000000000000000, 0.000000000000000000, 0.000000000000000000 ) ) ;
#11109 = CIRCLE ( 'NONE', #4933, 12.50000000000000178 ) ;
#11110 = CARTESIAN_POINT ( 'NONE',  ( 2.091802670701738531, 11.66854640885106953, 4.341499821985210339 ) ) ;
#11111 = ORIENTED_EDGE ( 'NONE', *, *, #12035, .F. ) ;
#11112 = CARTESIAN_POINT ( 'NONE',  ( -2.802233683753186266, 11.81444791271924899, -3.927002317657668051 ) ) ;
#11113 = CARTESIAN_POINT ( 'NONE',  ( -2.817565069457256932, 29.94682129341587284, 2.992080202207098694 ) ) ;
#11114 = AXIS2_PLACEMENT_3D ( 'NONE', #23290, #6466, #21001 ) ;
#11115 = CARTESIAN_POINT ( 'NONE',  ( 0.3124060177047779940, 29.44778486168719667, 2.256467045519745529 ) ) ;
#11116 = ORIENTED_EDGE ( 'NONE', *, *, #1584, .F. ) ;
#11117 = DIRECTION ( 'NONE',  ( 1.000000000000000000, 0.000000000000000000, 0.000000000000000000 ) ) ;
#11118 = CARTESIAN_POINT ( 'NONE',  ( 12.76143908531000193, 9.974460201879001175, 1.751222586102000101 ) ) ;
#11119 = CARTESIAN_POINT ( 'NONE',  ( 18.31564036859069233, 7.307524194310222043, -7.427871909705804576 ) ) ;
#11120 = ADVANCED_FACE ( 'NONE', ( #9667 ), #3442, .F. ) ;
#11121 = CARTESIAN_POINT ( 'NONE',  ( -5.372793533988000192, 16.07374366253000275, 2.940837684191000001 ) ) ;
#11122 = CARTESIAN_POINT ( 'NONE',  ( -0.2810990160142999295, 29.96038721557000173, -2.132306642366999849 ) ) ;
#11123 = DIRECTION ( 'NONE',  ( -1.000000000000000000, 0.000000000000000000, 0.000000000000000000 ) ) ;
#11124 = DIRECTION ( 'NONE',  ( -1.000000000000000000, 0.000000000000000000, 0.000000000000000000 ) ) ;
#11125 = ORIENTED_EDGE ( 'NONE', *, *, #4973, .T. ) ;
#11126 = CARTESIAN_POINT ( 'NONE',  ( -24.49594166687722208, 11.08137607230481869, 5.806427241679596563 ) ) ;
#11127 = CARTESIAN_POINT ( 'NONE',  ( 23.05164232683000236, -7.202366762678000356, 8.056812634288998964 ) ) ;
#11128 = PRODUCT ( 'Valve Operating Stem', 'Valve Operating Stem', '', ( #12443 ) ) ;
#11129 = CARTESIAN_POINT ( 'NONE',  ( 0.000000000000000000, 29.69999999999999929, 4.618802153517000519 ) ) ;
#11130 = VERTEX_POINT ( 'NONE', #8098 ) ;
#11131 = LINE ( 'NONE', #11011, #2659 ) ;
#11132 = CARTESIAN_POINT ( 'NONE',  ( -4.000000000000000000, 24.80000000000000426, -2.309401076759000304 ) ) ;
#11133 = CARTESIAN_POINT ( 'NONE',  ( -3.678206510409002483, 12.01686478324999818, 3.158609924971003124 ) ) ;
#11134 = CARTESIAN_POINT ( 'NONE',  ( 0.6632315864332809507, 29.16452115530013955, -2.086780444890731889 ) ) ;
#11135 = EDGE_CURVE ( 'NONE', #12183, #15471, #17182, .T. ) ;
#11136 = DIRECTION ( 'NONE',  ( -1.000000000000000000, 0.000000000000000000, 0.000000000000000000 ) ) ;
#11137 = EDGE_LOOP ( 'NONE', ( #13820, #5396, #5864, #20256, #17564, #22859, #20181, #6631 ) ) ;
#11138 = CARTESIAN_POINT ( 'NONE',  ( 66.60588651278291650, 35.51856778792605240, -1.000000000000000000 ) ) ;
#11139 = VERTEX_POINT ( 'NONE', #6264 ) ;
#11140 = CARTESIAN_POINT ( 'NONE',  ( -1.894396370449000111, 24.56827184614000004, -1.396035791950000160 ) ) ;
#11141 = CARTESIAN_POINT ( 'NONE',  ( 4.722551773131003827, 14.52147321335999663, 3.832747064962003680 ) ) ;
#11142 = CARTESIAN_POINT ( 'NONE',  ( 16.16483103379665920, 5.583924645481782356, 7.265765639378300556 ) ) ;
#11143 = CARTESIAN_POINT ( 'NONE',  ( -16.89534587121332621, -8.867923303744074559, 2.383057832484115401 ) ) ;
#11144 = VECTOR ( 'NONE', #14875, 1000.000000000000114 ) ;
#11145 = DIRECTION ( 'NONE',  ( -0.7071067811867959296, 0.7071067811862957742, 6.966833095770957245E-08 ) ) ;
#11146 = CARTESIAN_POINT ( 'NONE',  ( 15.94237658530999902, 1.989471272253999778, -10.01494924120000007 ) ) ;
#11147 =( LENGTH_UNIT ( ) NAMED_UNIT ( * ) SI_UNIT ( .MILLI., .METRE. ) );
#11148 = EDGE_LOOP ( 'NONE', ( #20333, #15624, #14071, #7032 ) ) ;
#11149 = CARTESIAN_POINT ( 'NONE',  ( -12.71102772709999940, -0.8480750162247000512, -9.618334173012000221 ) ) ;
#11150 = CARTESIAN_POINT ( 'NONE',  ( 0.000000000000000000, 29.85000000000000142, 0.000000000000000000 ) ) ;
#11151 = VECTOR ( 'NONE', #8854, 1000.000000000000000 ) ;
#11152 = CARTESIAN_POINT ( 'NONE',  ( 24.00016455292000117, -9.287173237304083173, 0.000000000000000000 ) ) ;
#11153 = EDGE_CURVE ( 'NONE', #12304, #5259, #11705, .T. ) ;
#11154 = VERTEX_POINT ( 'NONE', #7604 ) ;
#11155 = CARTESIAN_POINT ( 'NONE',  ( -21.01981106612999994, -10.46178610027000033, -4.064235816344999641 ) ) ;
#11156 = CARTESIAN_POINT ( 'NONE',  ( -2.298308792509000220, 24.40769234017999878, 0.4128243414548999901 ) ) ;
#11157 = CARTESIAN_POINT ( 'NONE',  ( 14.42251860313111500, -1.405275611345024434, -10.22176834447581228 ) ) ;
#11158 = AXIS2_PLACEMENT_3D ( 'NONE', #3614, #14397, #22458 ) ;
#11159 = DIRECTION ( 'NONE',  ( 0.000000000000000000, -0.8660254037844288266, -0.5000000000000169864 ) ) ;
#11160 = CARTESIAN_POINT ( 'NONE',  ( 22.36319398042000373, 10.93760387994999839, 2.659607438111999844 ) ) ;
#11161 = CARTESIAN_POINT ( 'NONE',  ( 2.366606196949999852, 30.23066102319999970, 0.9578807050024000791 ) ) ;
#11162 = CARTESIAN_POINT ( 'NONE',  ( 14.12090646444330488, 4.006132324064554773, 8.116375441945786307 ) ) ;
#11163 = DIRECTION ( 'NONE',  ( -0.000000000000000000, 1.000000000000000000, 0.000000000000000000 ) ) ;
#11164 = AXIS2_PLACEMENT_3D ( 'NONE', #10831, #18217, #1619 ) ;
#11165 = LINE ( 'NONE', #15248, #3671 ) ;
#11166 = EDGE_CURVE ( 'NONE', #17463, #3590, #1501, .T. ) ;
#11167 = CARTESIAN_POINT ( 'NONE',  ( 11.06626444615592320, 10.69977336184266115, -6.467440677431063101 ) ) ;
#11168 = VERTEX_POINT ( 'NONE', #15826 ) ;
#11169 = CARTESIAN_POINT ( 'NONE',  ( -2.480627735891629548, 24.20832311788705482, -0.5148137458739096006 ) ) ;
#11170 = CARTESIAN_POINT ( 'NONE',  ( 2.394884942776999814, 23.89488494277999919, 0.000000000000000000 ) ) ;
#11171 = ORIENTED_EDGE ( 'NONE', *, *, #8544, .F. ) ;
#11172 = CIRCLE ( 'NONE', #13097, 13.77250448648999637 ) ;
#11173 = CARTESIAN_POINT ( 'NONE',  ( 11.64696834793616098, -8.717038812755488308, -3.317893490969420434 ) ) ;
#11174 = DIRECTION ( 'NONE',  ( 1.000000000000000000, 0.000000000000000000, 0.000000000000000000 ) ) ;
#11175 = CARTESIAN_POINT ( 'NONE',  ( 22.24928936712999672, -9.242242329243000043, 0.000000000000000000 ) ) ;
#11176 = CIRCLE ( 'NONE', #1889, 3.000000000000000000 ) ;
#11177 = TOROIDAL_SURFACE ( 'NONE', #15407, 5.625000000000000000, 0.5000000000000000000 ) ;
#11178 = CARTESIAN_POINT ( 'NONE',  ( 16.10288977129999921, -0.1032177031646999976, -11.05906605220000039 ) ) ;
#11179 = FACE_BOUND ( 'NONE', #20405, .T. ) ;
#11180 = CARTESIAN_POINT ( 'NONE',  ( -0.7744564004552000336, 28.44212896666999768, 2.554499528901000183 ) ) ;
#11181 = ORIENTED_EDGE ( 'NONE', *, *, #11401, .T. ) ;
#11182 = ORIENTED_EDGE ( 'NONE', *, *, #23501, .F. ) ;
#11183 = CARTESIAN_POINT ( 'NONE',  ( -10.19985863876999943, 4.116323844992999526, 14.65115941988999992 ) ) ;
#11184 = AXIS2_PLACEMENT_3D ( 'NONE', #1036, #12191, #1287 ) ;
#11185 = CARTESIAN_POINT ( 'NONE',  ( -4.000000000000000000, 28.00000000000000000, 2.309401076759000304 ) ) ;
#11186 = DIRECTION ( 'NONE',  ( -1.000000000000000000, 0.000000000000000000, 0.000000000000000000 ) ) ;
#11187 = ADVANCED_FACE ( 'NONE', ( #19480 ), #308, .T. ) ;
#11188 = ORIENTED_EDGE ( 'NONE', *, *, #22137, .F. ) ;
#11189 = EDGE_CURVE ( 'NONE', #19119, #6273, #4952, .T. ) ;
#11190 = CARTESIAN_POINT ( 'NONE',  ( -14.46758738162251845, 11.92463202973721792, 4.345869468068095820 ) ) ;
#11191 = CARTESIAN_POINT ( 'NONE',  ( 20.96437270046331491, 2.410389349752802168, -8.969624798282467282 ) ) ;
#11192 = CARTESIAN_POINT ( 'NONE',  ( 6.241414926470116420, 13.66656409111985404, 1.744778710455607618 ) ) ;
#11193 = CARTESIAN_POINT ( 'NONE',  ( 16.19032491852358291, -3.051673150441691629, -9.904219964709449542 ) ) ;
#11194 = CARTESIAN_POINT ( 'NONE',  ( -17.50947430316999842, -10.99790399745999991, 1.405211504096999908 ) ) ;
#11195 = AXIS2_PLACEMENT_3D ( 'NONE', #7124, #22245, #18172 ) ;
#11196 = CARTESIAN_POINT ( 'NONE',  ( 0.1900786975556000014, 30.23224694295999981, 2.348537901832999708 ) ) ;
#11197 = AXIS2_PLACEMENT_3D ( 'NONE', #15915, #8433, #23426 ) ;
#11198 = CARTESIAN_POINT ( 'NONE',  ( -15.79874102787999846, 5.047191510808999304, 8.952058016012999886 ) ) ;
#11199 = CARTESIAN_POINT ( 'NONE',  ( 1.357139981220319980, 29.69016086971108948, 1.680935446004558687 ) ) ;
#11200 = EDGE_CURVE ( 'NONE', #12102, #13618, #4828, .T. ) ;
#11201 = ORIENTED_EDGE ( 'NONE', *, *, #13356, .T. ) ;
#11202 = CARTESIAN_POINT ( 'NONE',  ( -2.110330650965000387, 24.67076761794999840, 1.000962332422999923 ) ) ;
#11203 = EDGE_CURVE ( 'NONE', #21250, #11018, #20372, .T. ) ;
#11204 = CARTESIAN_POINT ( 'NONE',  ( 20.44111605004497534, 10.09892154715089596, 2.954736731020451757 ) ) ;
#11205 = CARTESIAN_POINT ( 'NONE',  ( 11.74999999482999868, 0.000000000000000000, 1.045589212608000028E-14 ) ) ;
#11206 = CIRCLE ( 'NONE', #2674, 7.000000000000000000 ) ;
#11207 = ORIENTED_EDGE ( 'NONE', *, *, #19952, .F. ) ;
#11208 = CARTESIAN_POINT ( 'NONE',  ( 12.52688711657000020, 7.716878364870000340, 11.63397459621999985 ) ) ;
#11209 = CARTESIAN_POINT ( 'NONE',  ( -4.018738216213002090, 13.61287253962000499, 4.587140350181000414 ) ) ;
#11210 = CARTESIAN_POINT ( 'NONE',  ( 0.000000000000000000, 22.09999988306816832, 0.000000000000000000 ) ) ;
#11211 = AXIS2_PLACEMENT_3D ( 'NONE', #5535, #14617, #12916 ) ;
#11212 = CARTESIAN_POINT ( 'NONE',  ( 13.91512625730999986, 8.379890869990997970, -3.647050788746000194 ) ) ;
#11213 = PRODUCT_DEFINITION_CONTEXT ( 'detailed design', #8513, 'design' ) ;
#11214 = ORIENTED_EDGE ( 'NONE', *, *, #5282, .F. ) ;
#11215 = AXIS2_PLACEMENT_3D ( 'NONE', #6562, #8385, #19774 ) ;
#11216 = CARTESIAN_POINT ( 'NONE',  ( -5.372793533988000192, 16.07374366253000275, 2.940837684191000001 ) ) ;
#11217 = CARTESIAN_POINT ( 'NONE',  ( -14.48633704289933810, 1.427546401368239293, -12.50000676666208221 ) ) ;
#11218 = ORIENTED_EDGE ( 'NONE', *, *, #20509, .F. ) ;
#11219 = B_SPLINE_CURVE_WITH_KNOTS ( 'NONE', 3,
 ( #9478, #258, #7663, #5952, #15037, #11541, #22433, #13226, #498, #20618 ),
 .UNSPECIFIED., .F., .F.,
 ( 4, 2, 2, 2, 4 ),
 ( 0.000000000000000000, 0.2500000000000001110, 0.5000000000000002220, 0.7500000000000001110, 1.000000000000000000 ),
 .UNSPECIFIED. ) ;
#11220 = DIRECTION ( 'NONE',  ( 0.000000000000000000, 0.000000000000000000, -1.000000000000000000 ) ) ;
#11221 = CARTESIAN_POINT ( 'NONE',  ( -4.798612374681999526, 12.63734946677000437, 0.4217961273138995937 ) ) ;
#11222 = CARTESIAN_POINT ( 'NONE',  ( -23.74237356432000112, -9.140086274078999651, -3.124721474173000058 ) ) ;
#11223 = CARTESIAN_POINT ( 'NONE',  ( 18.62128936713000371, -9.149140698829999252, 0.000000000000000000 ) ) ;
#11224 = CARTESIAN_POINT ( 'NONE',  ( -4.722737441090003152, 16.04185223773001923, -4.014586937476998685 ) ) ;
#11225 = CARTESIAN_POINT ( 'NONE',  ( -21.77107218145970080, 1.618043913735445205, 10.53815187480507198 ) ) ;
#11226 = CARTESIAN_POINT ( 'NONE',  ( 5.155714003469999973, 13.97328511022999997, 4.008150528822999270 ) ) ;
#11227 = DIRECTION ( 'NONE',  ( -0.8660254037844288266, 0.000000000000000000, 0.5000000000000169864 ) ) ;
#11228 = CARTESIAN_POINT ( 'NONE',  ( -6.410055968098999912, 15.31889920838999863, 1.282157099098000463 ) ) ;
#11229 =( BOUNDED_CURVE ( )  B_SPLINE_CURVE ( 3, ( #8729, #8605, #15967, #11100, #23361, #6779, #23490, #2483, #2606, #4065, #5990, #8061, #20901, #9752, #2240, #657 ),
 .UNSPECIFIED., .F., .F. ) 
 B_SPLINE_CURVE_WITH_KNOTS ( ( 4, 1, 1, 1, 1, 1, 1, 1, 1, 1, 1, 1, 1, 4 ),
 ( 0.000000000000000000, 0.002937754778506720781, 0.09205143729370196537, 0.1757691448987817595, 0.2560824178855284905, 0.3346853618078635129, 0.4126475807299391785, 0.4905595280248493117, 0.5689923879210118107, 0.6485670012755897496, 0.7300432222292638773, 0.8156447607010655076, 0.9090046746429836233, 1.000000000000000000 ),
 .UNSPECIFIED. ) 
 CURVE ( )  GEOMETRIC_REPRESENTATION_ITEM ( )  RATIONAL_B_SPLINE_CURVE ( ( 1.058246922893853581, 1.058246922893853581, 1.058246922893853581, 1.058246922893853581, 1.058246922893853581, 1.058246922893853581, 1.058246922893853581, 1.058246922893853581, 1.058246922893853581, 1.058246922893853581, 1.058246922893853581, 1.058246922893853581, 1.058246922893853581, 1.058246922893853581, 1.058246922893853581, 1.058246922893853581 ) ) 
 REPRESENTATION_ITEM ( '' )  );
#11230 = CARTESIAN_POINT ( 'NONE',  ( 2.018792404907182814, 30.65015847864969345, -0.7678982693529425863 ) ) ;
#11231 = ORIENTED_EDGE ( 'NONE', *, *, #23223, .F. ) ;
#11232 = CARTESIAN_POINT ( 'NONE',  ( -17.43032910583999850, 9.118578311265999048, 0.000000000000000000 ) ) ;
#11233 = CARTESIAN_POINT ( 'NONE',  ( 24.03948154624000111, -9.843283099998000552, -0.9867796264882999768 ) ) ;
#11234 = CARTESIAN_POINT ( 'NONE',  ( 0.9266888457184595529, 24.78564400243023869, 1.917495999108346894 ) ) ;
#11235 = CARTESIAN_POINT ( 'NONE',  ( -23.96454491813620180, 8.827218892942170214, -5.864176129446873276 ) ) ;
#11236 = CARTESIAN_POINT ( 'NONE',  ( 1.979460888490000015, 25.75437716036000069, 1.008585698963999855 ) ) ;
#11237 = CARTESIAN_POINT ( 'NONE',  ( 12.00000000000000000, -8.391897884961000642, -3.194141202603999918 ) ) ;
#11238 = FACE_OUTER_BOUND ( 'NONE', #21297, .T. ) ;
#11239 = EDGE_LOOP ( 'NONE', ( #22993, #6424, #10683, #6846 ) ) ;
#11240 = CARTESIAN_POINT ( 'NONE',  ( -0.08431463819058247766, 11.48104257302984088, -4.815429911517862038 ) ) ;
#11241 = CARTESIAN_POINT ( 'NONE',  ( 24.38510397947348096, 12.27045979993889802, 3.746940194273108204 ) ) ;
#11242 = CARTESIAN_POINT ( 'NONE',  ( 12.52688711657000020, -13.93375672974000068, 0.8660254037843999608 ) ) ;
#11243 = ORIENTED_EDGE ( 'NONE', *, *, #502, .F. ) ;
#11244 = CARTESIAN_POINT ( 'NONE',  ( 23.99478584078000054, -7.550251870592999737, 11.73017644753999988 ) ) ;
#11245 = CARTESIAN_POINT ( 'NONE',  ( 17.47800158530999681, -7.122204577229999778, -7.372745388647000020 ) ) ;
#11246 = CARTESIAN_POINT ( 'NONE',  ( 18.36750925429045012, 8.490495120173470411, -6.047999897081842491 ) ) ;
#11247 = CARTESIAN_POINT ( 'NONE',  ( -24.50000000000452971, 0.2564718131585235206, 12.50000000000233946 ) ) ;
#11248 = CARTESIAN_POINT ( 'NONE',  ( -1.380185735549000148, 29.23241029034999627, -1.649495554458999980 ) ) ;
#11249 = CARTESIAN_POINT ( 'NONE',  ( 14.51551537306000128, -5.756020581778999556, -9.120548154372999150 ) ) ;
#11250 = CARTESIAN_POINT ( 'NONE',  ( 13.50000000000000000, -5.669411096634266123, -7.227943221418801301 ) ) ;
#11251 = ORIENTED_EDGE ( 'NONE', *, *, #20156, .T. ) ;
#11252 = CARTESIAN_POINT ( 'NONE',  ( -23.74465998031000069, 13.93375672974000068, 0.8660254037843999608 ) ) ;
#11253 = CARTESIAN_POINT ( 'NONE',  ( 24.11393693976000208, 10.34077239664000025, -3.237760962710000356 ) ) ;
#11254 = CARTESIAN_POINT ( 'NONE',  ( 1.536366799937303407, 29.08333333333333215, 1.999167105995437677 ) ) ;
#11255 = ORIENTED_EDGE ( 'NONE', *, *, #15088, .T. ) ;
#11256 = CARTESIAN_POINT ( 'NONE',  ( -12.49016237973315313, 6.849135750923734278, -5.827197512145549929 ) ) ;
#11257 = CYLINDRICAL_SURFACE ( 'NONE', #997, 2.000000000000000000 ) ;
#11258 = CIRCLE ( 'NONE', #13556, 4.724999999999999645 ) ;
#11259 = CARTESIAN_POINT ( 'NONE',  ( 3.786219791712002625, 12.04888752014999653, 3.147501422329002096 ) ) ;
#11260 = B_SPLINE_CURVE_WITH_KNOTS ( 'NONE', 3,
 ( #8092, #19222, #15692, #2763, #4706, #12331, #2634, #15936, #17415, #6743 ),
 .UNSPECIFIED., .F., .F.,
 ( 4, 1, 1, 2, 2, 4 ),
 ( 0.000000000000000000, 0.2499999999999994449, 0.3749999999999989453, 0.4374999999999987788, 0.4999999999999985567, 1.000000000000000000 ),
 .UNSPECIFIED. ) ;
#11261 = CARTESIAN_POINT ( 'NONE',  ( -0.3748402411544077273, 29.22614913440824935, -2.127372941641080040 ) ) ;
#11262 = CARTESIAN_POINT ( 'NONE',  ( -19.63740412539999980, 1.666533117798999930, 10.91439899677999925 ) ) ;
#11263 = ORIENTED_EDGE ( 'NONE', *, *, #3356, .F. ) ;
#11264 = DIRECTION ( 'NONE',  ( 0.000000000000000000, 0.000000000000000000, -1.000000000000000000 ) ) ;
#11265 = ORIENTED_EDGE ( 'NONE', *, *, #6447, .T. ) ;
#11266 = ADVANCED_FACE ( 'NONE', ( #7343 ), #5301, .T. ) ;
#11267 = CARTESIAN_POINT ( 'NONE',  ( -0.2356110571030000100, 23.66255821230999956, -2.226257962701000181 ) ) ;
#11268 = CARTESIAN_POINT ( 'NONE',  ( 0.3272492347489455167, 28.21666666666666856, 2.499999999999998668 ) ) ;
#11269 = CARTESIAN_POINT ( 'NONE',  ( -0.6576354733792000307, 28.65299822781000216, 2.169172474974999876 ) ) ;
#11270 = CYLINDRICAL_SURFACE ( 'NONE', #1060, 4.750000000000000000 ) ;
#11271 = DIRECTION ( 'NONE',  ( -1.000000000000000000, 0.000000000000000000, 0.000000000000000000 ) ) ;
#11272 = DIRECTION ( 'NONE',  ( 0.000000000000000000, 1.000000000000000000, 0.000000000000000000 ) ) ;
#11273 = CARTESIAN_POINT ( 'NONE',  ( -3.100000000000000089, 17.00000000000000000, 0.000000000000000000 ) ) ;
#11274 = CARTESIAN_POINT ( 'NONE',  ( -15.75798294665000121, 9.136783202530001091, 3.374990494159999965 ) ) ;
#11275 = FACE_OUTER_BOUND ( 'NONE', #9347, .T. ) ;
#11276 = FACE_OUTER_BOUND ( 'NONE', #21024, .T. ) ;
#11277 = ORIENTED_EDGE ( 'NONE', *, *, #14312, .F. ) ;
#11278 = EDGE_CURVE ( 'NONE', #12315, #889, #6516, .T. ) ;
#11279 = CARTESIAN_POINT ( 'NONE',  ( -20.33434412369999933, 10.33430737248000142, -4.330206088669999787 ) ) ;
#11280 = CARTESIAN_POINT ( 'NONE',  ( -1.285289189667999876, 23.80867471234000021, 1.716809468418999840 ) ) ;
#11281 = CARTESIAN_POINT ( 'NONE',  ( 13.86150418236414161, -8.974767284217415764, 5.068416743520222312 ) ) ;
#11282 = CARTESIAN_POINT ( 'NONE',  ( 0.000000000000000000, 21.95000012746600149, -4.699999872533999756 ) ) ;
#11283 = CARTESIAN_POINT ( 'NONE',  ( 20.56464971682999732, 7.808581107292000389, 8.038765694828999386 ) ) ;
#11284 = CARTESIAN_POINT ( 'NONE',  ( 1.736698740103000071, 29.58438105280999864, -1.871426636120000042 ) ) ;
#11285 = CARTESIAN_POINT ( 'NONE',  ( 13.69363924190391302, 8.424036582202942824, -3.228120261996942908 ) ) ;
#11286 = CARTESIAN_POINT ( 'NONE',  ( -6.281974597825559670, 15.68480551511767729, -1.218664578910494400 ) ) ;
#11287 = DIRECTION ( 'NONE',  ( 1.000000000000000000, 0.000000000000000000, 0.000000000000000000 ) ) ;
#11288 = CARTESIAN_POINT ( 'NONE',  ( 11.39490977864222998, 9.382231423120625635, -8.749413452953497483 ) ) ;
#11289 = ORIENTED_EDGE ( 'NONE', *, *, #23265, .T. ) ;
#11290 = CARTESIAN_POINT ( 'NONE',  ( -0.3439877393419937257, 24.41664673104403960, 2.509216680981930736 ) ) ;
#11291 = DIRECTION ( 'NONE',  ( 0.000000000000000000, 0.000000000000000000, 1.000000000000000000 ) ) ;
#11292 = EDGE_LOOP ( 'NONE', ( #19001, #3549, #22711 ) ) ;
#11293 = ADVANCED_FACE ( 'NONE', ( #12911 ), #20308, .F. ) ;
#11294 = CARTESIAN_POINT ( 'NONE',  ( -1.750000000000000000, 9.000000000000000000, 0.000000000000000000 ) ) ;
#11295 = VECTOR ( 'NONE', #20648, 1000.000000000000114 ) ;
#11296 = CARTESIAN_POINT ( 'NONE',  ( 0.000000000000000000, 21.50000000000000000, 0.000000000000000000 ) ) ;
#11297 = CARTESIAN_POINT ( 'NONE',  ( 24.19085492956958561, -9.549256642876626344, 0.0002501093553063627687 ) ) ;
#11298 = CARTESIAN_POINT ( 'NONE',  ( 16.06906047033999840, -6.554063206097999306, -8.907152100438999298 ) ) ;
#11299 = DIRECTION ( 'NONE',  ( 0.000000000000000000, -1.000000000000000000, 0.000000000000000000 ) ) ;
#11300 = CARTESIAN_POINT ( 'NONE',  ( 2.437990915149000237, 25.45212896666999924, 0.5485649090615000167 ) ) ;
#11301 = VERTEX_POINT ( 'NONE', #7221 ) ;
#11302 = ORIENTED_EDGE ( 'NONE', *, *, #18897, .T. ) ;
#11303 = CARTESIAN_POINT ( 'NONE',  ( 0.3272492347489341924, 27.21753006952334530, -2.500000000000000888 ) ) ;
#11304 = CARTESIAN_POINT ( 'NONE',  ( 1.750000000000000000, 7.000000000000000000, 0.000000000000000000 ) ) ;
#11305 = B_SPLINE_CURVE_WITH_KNOTS ( 'NONE', 3,
 ( #5433, #3967, #14622, #2026, #14738, #22480, #16786, #7353 ),
 .UNSPECIFIED., .F., .F.,
 ( 4, 2, 2, 4 ),
 ( 0.000000000000000000, 0.2500000000000002220, 0.5000000000000004441, 1.000000000000000000 ),
 .UNSPECIFIED. ) ;
#11306 = DIRECTION ( 'NONE',  ( -2.971992933571787233E-05, -0.9999999995583628287, -8.164609096927661075E-09 ) ) ;
#11307 = VERTEX_POINT ( 'NONE', #9168 ) ;
#11308 = ADVANCED_FACE ( 'NONE', ( #5189 ), #23919, .T. ) ;
#11309 = CARTESIAN_POINT ( 'NONE',  ( -14.37382028566454650, 13.01774735372515046, 2.452106660089753642 ) ) ;
#11310 = CARTESIAN_POINT ( 'NONE',  ( 19.88201599663697294, 5.989684672267420851, -8.637120499181696331 ) ) ;
#11311 = CARTESIAN_POINT ( 'NONE',  ( 21.45754691133435799, 36.29044427405532502, -115.0195023120000002 ) ) ;
#11312 = CARTESIAN_POINT ( 'NONE',  ( 16.01801534404138394, -8.067232948202645915, -6.498016440650728143 ) ) ;
#11313 = CARTESIAN_POINT ( 'NONE',  ( -19.43654966351000013, -9.242645412567998875, 5.313552282507999713 ) ) ;
#11314 = CARTESIAN_POINT ( 'NONE',  ( 1.433070709896999917, 29.72363129601999887, 1.653766674786000035 ) ) ;
#11315 = AXIS2_PLACEMENT_3D ( 'NONE', #16854, #22545, #14795 ) ;
#11316 = CARTESIAN_POINT ( 'NONE',  ( -16.04262945707999677, 5.313593037366000082, 9.424424275870000756 ) ) ;
#11317 = ADVANCED_FACE ( 'NONE', ( #14383 ), #12805, .T. ) ;
#11318 = CARTESIAN_POINT ( 'NONE',  ( 0.4639490188554213912, 29.63126733662222989, 2.109472460375426017 ) ) ;
#11319 = ORIENTED_EDGE ( 'NONE', *, *, #22567, .F. ) ;
#11320 = CARTESIAN_POINT ( 'NONE',  ( 1.450318268071000061, 24.34012059315000087, -1.629560560109000189 ) ) ;
#11321 = CARTESIAN_POINT ( 'NONE',  ( 2.999999956181000016, 17.90000004382000043, -2.609181548331000199E-08 ) ) ;
#11322 = CARTESIAN_POINT ( 'NONE',  ( -17.93571553221221393, -5.561216854535629750, 8.842563169821765712 ) ) ;
#11323 = VERTEX_POINT ( 'NONE', #21777 ) ;
#11324 = EDGE_CURVE ( 'NONE', #15568, #2993, #3713, .T. ) ;
#11325 = CARTESIAN_POINT ( 'NONE',  ( 24.18393254356892896, -4.886968879243103636, 12.50000000000000178 ) ) ;
#11326 = CARTESIAN_POINT ( 'NONE',  ( -3.428088622465001567, 14.04569531913998937, 5.080072178502000213 ) ) ;
#11327 = EDGE_CURVE ( 'NONE', #20695, #13697, #19959, .T. ) ;
#11328 = FACE_OUTER_BOUND ( 'NONE', #15768, .T. ) ;
#11329 = CARTESIAN_POINT ( 'NONE',  ( 16.68375142130999933, -4.435783964195000095, 8.649968580473998969 ) ) ;
#11330 = EDGE_LOOP ( 'NONE', ( #4247, #21867, #5177, #5139 ) ) ;
#11331 = B_SPLINE_CURVE_WITH_KNOTS ( 'NONE', 3,
 ( #16818, #20124, #11026, #22161 ),
 .UNSPECIFIED., .F., .F.,
 ( 4, 4 ),
 ( 0.000000000000000000, 1.000000000000000000 ),
 .UNSPECIFIED. ) ;
#11332 = AXIS2_PLACEMENT_3D ( 'NONE', #11902, #2699, #10202 ) ;
#11333 = CARTESIAN_POINT ( 'NONE',  ( -4.632252426630697251, 15.60046821123447813, 4.007232082546550167 ) ) ;
#11334 = FACE_OUTER_BOUND ( 'NONE', #14910, .T. ) ;
#11335 = B_SPLINE_SURFACE_WITH_KNOTS ( 'NONE', 3, 3, ( 
 ( #114, #9684, #9799, #19375, #8232, #2784, #22627, #2657, #22868, #22747, #10052, #462, #4240, #12112, #6530, #21187, #11862, #706, #9920, #17064, #13666, #11629, #19498, #829, #17435, #20826, #11990, #17185, #18999, #6403, #13915, #4353, #10170, #951, #7865, #15233, #2409, #6038, #15599, #17307, #13426, #580, #19116, #17555, #7985, #15357, #4724, #13550, #8350, #8117, #22986, #13785, #15482, #15714, #21311, #4601, #6282, #6165, #23106, #20946, #11743, #21059, #2530, #4473, #19246, #15842, #10416 ),
 ( #1076, #17807, #5316, #23231, #19744, #3393, #8956, #16080, #1447, #8843, #12355, #15957, #23350, #3154, #10537, #12706, #8594, #21790, #17922, #7121, #3271, #21905, #8475, #1203, #16324, #6768, #14511, #2907, #1327, #23605, #10654, #14040, #6644, #18169, #12233, #19620, #10777, #21678, #14161, #23715, #21556, #10289, #4970, #8716, #14283, #23479, #5090, #6890, #7010, #18042, #16208, #17678, #21433, #4846, #3029, #12470, #19856, #14398, #5205, #12587, #19974, #1572, #22024, #3509, #18623, #16913, #23827 ),
 ( #10890, #317, #7357, #7722, #22135, #7236, #16790, #7591, #18736, #5437, #16560, #18384, #14742, #11245, #18276, #1675, #2030, #12818, #15087, #20440, #9303, #20211, #9065, #3616, #3852, #5546, #14970, #12924, #22484, #5893, #7469, #20098, #16436, #14627, #9420, #85, #5782, #10999, #1795, #20321, #14854, #198, #5659, #3729, #9183, #1914, #22242, #22368, #13166, #20556, #13044, #3970, #11363, #2143, #23950, #9537, #11118, #18504, #16677, #20678, #8322, #17158, #11962, #4325, #6252, #17410, #11716 ),
 ( #4570, #2758, #13636, #9890, #9657, #19351, #4086, #13756, #15453, #17038, #8204, #19088, #2502, #22840, #11481, #4208, #15687, #2263, #6132, #21159, #10139, #17280, #11836, #19217, #22720, #2382, #9771, #13523, #20920, #23077, #18974, #15570, #680, #17528, #21031, #13279, #18858, #20797, #920, #553, #435, #7837, #8087, #10025, #4446, #15207, #22604, #6012, #13398, #11601, #7958, #2629, #15331, #803, #22958, #6375, #10387, #12326, #17897, #21402, #1298, #1178, #10629, #21652, #5065, #19947, #2877 ) ),
 .UNSPECIFIED., .F., .F., .F.,
 ( 4, 4 ),
 ( 4, 1, 1, 1, 1, 1, 1, 1, 1, 1, 1, 1, 1, 1, 1, 1, 1, 1, 1, 1, 1, 1, 1, 1, 1, 1, 1, 1, 1, 1, 1, 1, 1, 1, 1, 1, 1, 1, 1, 1, 1, 1, 1, 1, 1, 1, 1, 1, 1, 1, 1, 1, 1, 1, 1, 1, 1, 1, 1, 1, 1, 1, 1, 1, 4 ),
 ( -0.08331297109794000288, 1.083312971098000066 ),
 ( -0.02000000000000000042, -0.003749999999999999861, 0.01250000000000000069, 0.02875000000000000125, 0.04499999999999999833, 0.06124999999999999889, 0.07749999999999999944, 0.09375000000000000000, 0.1100000000000000006, 0.1262500000000000011, 0.1424999999999999878, 0.1587500000000000022, 0.1749999999999999889, 0.1912500000000000033, 0.2074999999999999900, 0.2237500000000000044, 0.2399999999999999911, 0.2562499999999999778, 0.2725000000000000200, 0.2887500000000000067, 0.3049999999999999933, 0.3212499999999999800, 0.3375000000000000222, 0.3537500000000000089, 0.3699999999999999956, 0.3862499999999999822, 0.4025000000000000244, 0.4187500000000000111, 0.4349999999999999978, 0.4512499999999999845, 0.4675000000000000266, 0.4837500000000000133, 0.5000000000000000000, 0.5162499999999999867, 0.5324999999999999734, 0.5487499999999999600, 0.5649999999999999467, 0.5812500000000000444, 0.5975000000000000311, 0.6137500000000000178, 0.6300000000000000044, 0.6462499999999999911, 0.6624999999999999778, 0.6787499999999999645, 0.6949999999999999512, 0.7112500000000000488, 0.7275000000000000355, 0.7437500000000000222, 0.7600000000000000089, 0.7762499999999999956, 0.7924999999999999822, 0.8087499999999999689, 0.8249999999999999556, 0.8412500000000000533, 0.8575000000000000400, 0.8737500000000000266, 0.8900000000000000133, 0.9062500000000000000, 0.9224999999999999867, 0.9387499999999999734, 0.9549999999999999600, 0.9712499999999999467, 0.9875000000000000444, 1.003749999999999920, 1.020000000000000018 ),
 .UNSPECIFIED. ) ;
#11336 = VERTEX_POINT ( 'NONE', #8827 ) ;
#11337 = EDGE_CURVE ( 'NONE', #15685, #5518, #17482, .T. ) ;
#11338 = CARTESIAN_POINT ( 'NONE',  ( 22.89174770046333407, 5.689831819425626769, -7.403988410609271931 ) ) ;
#11339 = CARTESIAN_POINT ( 'NONE',  ( -4.593072733376997618, 12.55937666042000345, 1.460090207240998694 ) ) ;
#11340 = CARTESIAN_POINT ( 'NONE',  ( -20.85181323488999894, 5.829520124619999244, 7.603889561582000134 ) ) ;
#11341 = CARTESIAN_POINT ( 'NONE',  ( -14.45561362881575462, 9.532958125092610757, -8.488361093004769486 ) ) ;
#11342 = CARTESIAN_POINT ( 'NONE',  ( -4.676113636882003100, 15.28248474626999531, -3.572242236667999560 ) ) ;
#11343 = DIRECTION ( 'NONE',  ( 0.000000000000000000, 1.000000000000000000, 0.000000000000000000 ) ) ;
#11344 = CARTESIAN_POINT ( 'NONE',  ( 2.399999988617999680, 29.99999998861800066, 6.349992443878999481E-08 ) ) ;
#11345 = CARTESIAN_POINT ( 'NONE',  ( 0.4139582100457485092, 30.42833226141065595, 2.119867715313618728 ) ) ;
#11346 = EDGE_LOOP ( 'NONE', ( #12776, #13917, #4581 ) ) ;
#11347 = CARTESIAN_POINT ( 'NONE',  ( -17.39253743917333495, 9.117608502615587085, 1.193619109743944584 ) ) ;
#11348 = CARTESIAN_POINT ( 'NONE',  ( 19.98121194148999891, -1.753880888304999885, 9.622565653743999192 ) ) ;
#11349 = CARTESIAN_POINT ( 'NONE',  ( 1.607383496580327087, 24.77257767849905079, 1.394007648165144664 ) ) ;
#11350 =( GEOMETRIC_REPRESENTATION_CONTEXT ( 3 ) GLOBAL_UNCERTAINTY_ASSIGNED_CONTEXT ( ( #10892 ) ) GLOBAL_UNIT_ASSIGNED_CONTEXT ( ( #22052, #7624, #18534 ) ) REPRESENTATION_CONTEXT ( 'NONE', 'WORKASPACE' ) );
#11351 = DIRECTION ( 'NONE',  ( 0.000000000000000000, 0.000000000000000000, 1.000000000000000000 ) ) ;
#11352 = CARTESIAN_POINT ( 'NONE',  ( -24.01809766817718739, 7.654457563781243756, -7.454922064010741423 ) ) ;
#11353 = CARTESIAN_POINT ( 'NONE',  ( 0.5279260092677000582, 28.19446440325999959, -2.406140597653999791 ) ) ;
#11354 = CARTESIAN_POINT ( 'NONE',  ( -6.000000000000000000, 24.99999999999999645, -115.0195023120000002 ) ) ;
#11355 = ORIENTED_EDGE ( 'NONE', *, *, #11615, .F. ) ;
#11356 = CARTESIAN_POINT ( 'NONE',  ( -0.8888509597944463936, 11.51654473730785888, -4.729873641147137597 ) ) ;
#11357 = CARTESIAN_POINT ( 'NONE',  ( 24.48327518124253643, 11.46871523476161059, 5.135602515852324856 ) ) ;
#11358 = DIRECTION ( 'NONE',  ( 0.000000000000000000, -1.000000000000000000, 0.000000000000000000 ) ) ;
#11359 = ORIENTED_EDGE ( 'NONE', *, *, #3636, .T. ) ;
#11360 = EDGE_CURVE ( 'NONE', #21466, #20461, #14278, .T. ) ;
#11361 = CARTESIAN_POINT ( 'NONE',  ( -8.035714285714000482, 1.323055916935999825E-14, 0.000000000000000000 ) ) ;
#11362 = ADVANCED_FACE ( 'NONE', ( #21663 ), #5076, .F. ) ;
#11363 = CARTESIAN_POINT ( 'NONE',  ( 13.20018908531000079, -1.240977706124000157, 10.06232283554999896 ) ) ;
#11364 = FACE_OUTER_BOUND ( 'NONE', #14030, .T. ) ;
#11365 = DIRECTION ( 'NONE',  ( -0.000000000000000000, 1.000000000000000000, 0.000000000000000000 ) ) ;
#11366 = CARTESIAN_POINT ( 'NONE',  ( 13.49989037305999950, 8.681618249821999811, 6.350899454929000321 ) ) ;
#11367 = AXIS2_PLACEMENT_3D ( 'NONE', #4411, #11449, #20762 ) ;
#11368 = DIRECTION ( 'NONE',  ( -0.9996708941621502698, -0.02565352539217870959, -3.571920101197821240E-14 ) ) ;
#11369 = FACE_BOUND ( 'NONE', #1266, .T. ) ;
#11370 = CARTESIAN_POINT ( 'NONE',  ( 23.06310416476999592, 8.733239352628999086, 4.332342072756000029 ) ) ;
#11371 = AXIS2_PLACEMENT_3D ( 'NONE', #13882, #6980, #15684 ) ;
#11372 = DIRECTION ( 'NONE',  ( 1.000000000000000000, 0.000000000000000000, 0.000000000000000000 ) ) ;
#11373 = ORIENTED_EDGE ( 'NONE', *, *, #13978, .F. ) ;
#11374 = CARTESIAN_POINT ( 'NONE',  ( 11.89873226653999794, -8.042551475384998483, -4.234871351403000084 ) ) ;
#11375 = FACE_OUTER_BOUND ( 'NONE', #13605, .T. ) ;
#11376 = CARTESIAN_POINT ( 'NONE',  ( 2.369987487222001032, 11.69121506501000951, 4.325025584672001600 ) ) ;
#11377 = CARTESIAN_POINT ( 'NONE',  ( -1.234859021521087730, 29.28134306420319888, -1.772094427844483455 ) ) ;
#11378 = CARTESIAN_POINT ( 'NONE',  ( -24.60901460102000016, -6.746808026584999674, -8.909132170008000173 ) ) ;
#11379 = ORIENTED_EDGE ( 'NONE', *, *, #9850, .T. ) ;
#11380 = CARTESIAN_POINT ( 'NONE',  ( -18.73259798496000172, -8.620928137991000995, 3.072238420002000314 ) ) ;
#11381 = VERTEX_POINT ( 'NONE', #9404 ) ;
#11382 = CIRCLE ( 'NONE', #2878, 3.100000000000000089 ) ;
#11383 = CARTESIAN_POINT ( 'NONE',  ( -2.316775158635999698, 23.87156905088000158, 0.4125208335121000602 ) ) ;
#11384 = CARTESIAN_POINT ( 'NONE',  ( 5.091363865865001337, 14.05312055460999687, 3.675988761441002062 ) ) ;
#11385 = CARTESIAN_POINT ( 'NONE',  ( 2.266578917753999889, 27.28799822781000017, 0.04450989311242999763 ) ) ;
#11386 = CARTESIAN_POINT ( 'NONE',  ( 16.27820603379666409, 2.379147093495555421, 8.852401313026854623 ) ) ;
#11387 = DIRECTION ( 'NONE',  ( 0.000000000000000000, 0.000000000000000000, 1.000000000000000000 ) ) ;
#11388 = CARTESIAN_POINT ( 'NONE',  ( 23.99062354302999722, 6.216878364870000340, 12.50000000000000000 ) ) ;
#11389 = CIRCLE ( 'NONE', #1725, 15.45000000000000107 ) ;
#11390 = CARTESIAN_POINT ( 'NONE',  ( -12.54865546036000090, 9.084388929069001861, -2.336084003038000123 ) ) ;
#11391 = B_SPLINE_CURVE_WITH_KNOTS ( 'NONE', 3,
 ( #9817, #9578, #23002, #19262, #22884, #5934, #478, #2185, #8132, #6298, #22527, #2677, #10066, #13321, #17451, #844, #4367, #8247 ),
 .UNSPECIFIED., .F., .F.,
 ( 4, 2, 2, 2, 2, 2, 2, 2, 4 ),
 ( 0.000000000000000000, 0.1250000000000000555, 0.2500000000000000555, 0.3750000000000000555, 0.5000000000000000000, 0.6249999999999998890, 0.7499999999999998890, 0.8749999999999998890, 1.000000000000000000 ),
 .UNSPECIFIED. ) ;
#11392 = CARTESIAN_POINT ( 'NONE',  ( 4.000000000000000000, 29.93562577624027199, 1.040161751118763078 ) ) ;
#11393 = DIRECTION ( 'NONE',  ( 0.000000000000000000, -1.000000000000000000, 0.000000000000000000 ) ) ;
#11394 = VERTEX_POINT ( 'NONE', #22589 ) ;
#11395 = CARTESIAN_POINT ( 'NONE',  ( 12.50000000000000000, -13.93375672974000068, -0.1443160066108999939 ) ) ;
#11396 = CARTESIAN_POINT ( 'NONE',  ( 1.575558360453000128, 24.45298753663999847, 2.212366420454999982 ) ) ;
#11397 = CARTESIAN_POINT ( 'NONE',  ( 14.21677320012310020, -7.733754170777608294, -6.825353183793160028 ) ) ;
#11398 = AXIS2_PLACEMENT_3D ( 'NONE', #19065, #9868, #8056 ) ;
#11399 = CARTESIAN_POINT ( 'NONE',  ( 0.000000000000000000, 22.19999999999999574, 0.000000000000000000 ) ) ;
#11400 = CARTESIAN_POINT ( 'NONE',  ( 18.94965241622000107, -4.614544171587000143, 10.16351295409999977 ) ) ;
#11401 = EDGE_CURVE ( 'NONE', #10250, #7057, #16599, .T. ) ;
#11402 = CARTESIAN_POINT ( 'NONE',  ( -2.552764028111999650, 29.08171885361999998, 0.04190466168120000195 ) ) ;
#11403 = CARTESIAN_POINT ( 'NONE',  ( 14.40647345916092270, -4.520956232057431023, 7.829320738539829350 ) ) ;
#11404 = CARTESIAN_POINT ( 'NONE',  ( 24.24531177150999994, 0.000000000000000000, 0.000000000000000000 ) ) ;
#11405 = LINE ( 'NONE', #16963, #17999 ) ;
#11406 = CARTESIAN_POINT ( 'NONE',  ( 12.06371966925150829, 8.266677038032856473, -10.68189384366227479 ) ) ;
#11407 = ORIENTED_EDGE ( 'NONE', *, *, #1640, .F. ) ;
#11408 = CARTESIAN_POINT ( 'NONE',  ( 12.04708237233491275, -13.35071834206843988, 1.875975938905986684 ) ) ;
#11409 = ORIENTED_EDGE ( 'NONE', *, *, #18729, .T. ) ;
#11410 = CARTESIAN_POINT ( 'NONE',  ( -16.33437077250664515, -7.269244768974109761, -5.586598368547599058 ) ) ;
#11411 = DIRECTION ( 'NONE',  ( -1.000000000000000000, 0.000000000000000000, 0.000000000000000000 ) ) ;
#11412 = CARTESIAN_POINT ( 'NONE',  ( -23.75391248683000356, -6.466663555194999802, -12.35578645312999946 ) ) ;
#11413 = ORIENTED_EDGE ( 'NONE', *, *, #6136, .F. ) ;
#11414 = VECTOR ( 'NONE', #4002, 1000.000000000000114 ) ;
#11415 = CARTESIAN_POINT ( 'NONE',  ( 16.24951136818999942, -0.1032548074114000153, -11.06308154020999979 ) ) ;
#11416 = CARTESIAN_POINT ( 'NONE',  ( 0.000000000000000000, 26.50000000000000355, 0.000000000000000000 ) ) ;
#11417 = CARTESIAN_POINT ( 'NONE',  ( -2.505154520421000175, 28.23919433610000240, 1.402946323589000066 ) ) ;
#11418 = VERTEX_POINT ( 'NONE', #20905 ) ;
#11419 = EDGE_LOOP ( 'NONE', ( #2111, #469, #22619, #1534, #23017, #21440 ) ) ;
#11420 = CARTESIAN_POINT ( 'NONE',  ( 23.99062354302999722, 13.93375672974000068, 0.8660254037843999608 ) ) ;
#11421 = CARTESIAN_POINT ( 'NONE',  ( 2.500000000000000000, 27.05086340285665969, -0.3272492347489373565 ) ) ;
#11422 = FACE_OUTER_BOUND ( 'NONE', #8158, .T. ) ;
#11423 = FACE_OUTER_BOUND ( 'NONE', #13461, .T. ) ;
#11424 = ORIENTED_EDGE ( 'NONE', *, *, #805, .T. ) ;
#11425 = CARTESIAN_POINT ( 'NONE',  ( 20.01733333333332965, -8.274956899206415528, 4.125424567703399603 ) ) ;
#11426 = CARTESIAN_POINT ( 'NONE',  ( 21.30449770046331182, 9.217997112989703368, -1.206759948112940517 ) ) ;
#11427 = CARTESIAN_POINT ( 'NONE',  ( 6.190159225257540143, 13.92116770842173779, 0.7872319910898135653 ) ) ;
#11428 = CARTESIAN_POINT ( 'NONE',  ( 15.67523878052337238, -9.013036842459623443, 5.090761818925328974 ) ) ;
#11429 = CARTESIAN_POINT ( 'NONE',  ( -14.79952457769999974, 10.86285964459999853, -1.812798036683000102 ) ) ;
#11430 = ADVANCED_FACE ( 'NONE', ( #13028 ), #5767, .F. ) ;
#11431 = CARTESIAN_POINT ( 'NONE',  ( -0.3402753032406000133, 28.56835218490999750, 2.088129448976000280 ) ) ;
#11432 = CIRCLE ( 'NONE', #19564, 13.93375672974000068 ) ;
#11433 = CARTESIAN_POINT ( 'NONE',  ( -14.37682859208999986, 9.777980407524001549, -3.031781461267000211 ) ) ;
#11434 = CARTESIAN_POINT ( 'NONE',  ( 1.421375682288115838, 29.69513268992620780, 1.626398583794437691 ) ) ;
#11435 = EDGE_LOOP ( 'NONE', ( #12891, #5074 ) ) ;
#11436 = CARTESIAN_POINT ( 'NONE',  ( -24.50000000000000000, -1.873582633960999999, -10.39897383761999983 ) ) ;
#11437 = CARTESIAN_POINT ( 'NONE',  ( -19.26691752923823486, -8.287860411292584217, -6.431204527717159891 ) ) ;
#11438 = VERTEX_POINT ( 'NONE', #22704 ) ;
#11439 = DIRECTION ( 'NONE',  ( -1.000000000000000000, 0.000000000000000000, 0.000000000000000000 ) ) ;
#11440 = CARTESIAN_POINT ( 'NONE',  ( -4.278150909564998550, 14.58147911605000679, 4.161691560141001389 ) ) ;
#11441 = ADVANCED_FACE ( 'NONE', ( #9756 ), #6303, .F. ) ;
#11442 = CARTESIAN_POINT ( 'NONE',  ( -3.000000000000000000, 22.00000000000000000, 0.000000000000000000 ) ) ;
#11443 = VECTOR ( 'NONE', #15041, 1000.000000000000114 ) ;
#11444 = CARTESIAN_POINT ( 'NONE',  ( 18.00000142131000302, 9.258615172493000145, 3.074095935696000037 ) ) ;
#11445 = ORIENTED_EDGE ( 'NONE', *, *, #8012, .T. ) ;
#11446 = CIRCLE ( 'NONE', #7184, 7.000000000000000000 ) ;
#11447 = CARTESIAN_POINT ( 'NONE',  ( -11.00000000000000000, 7.000000000000000000, 0.000000000000000000 ) ) ;
#11448 = EDGE_CURVE ( 'NONE', #4536, #8569, #7655, .T. ) ;
#11449 = DIRECTION ( 'NONE',  ( 0.000000000000000000, -1.000000000000000000, 0.000000000000000000 ) ) ;
#11450 = ORIENTED_EDGE ( 'NONE', *, *, #19897, .T. ) ;
#11451 = CARTESIAN_POINT ( 'NONE',  ( -16.63080420454665287, -7.275327887506832347, -5.591273266071538295 ) ) ;
#11452 = CARTESIAN_POINT ( 'NONE',  ( -12.50000000000000000, 6.965460728298000781, -5.686777139159000072 ) ) ;
#11453 = CARTESIAN_POINT ( 'NONE',  ( 2.851731227921999512, 12.01786460732001238, 3.895295054763002973 ) ) ;
#11454 = CARTESIAN_POINT ( 'NONE',  ( 12.00000000000000178, -4.124037653275831161, -8.674183391547163779 ) ) ;
#11455 = EDGE_CURVE ( 'NONE', #23934, #15484, #9935, .T. ) ;
#11456 = CARTESIAN_POINT ( 'NONE',  ( 19.37712270046332463, 8.011294138967238965, -4.617566475226050571 ) ) ;
#11457 = LINE ( 'NONE', #5988, #23161 ) ;
#11458 = CARTESIAN_POINT ( 'NONE',  ( 1.830943384928172435, 26.42105733796857692, -1.434664342410846505 ) ) ;
#11459 = CARTESIAN_POINT ( 'NONE',  ( 1.536366799937286087, 28.75086340285666608, -1.999167105995451221 ) ) ;
#11460 = CARTESIAN_POINT ( 'NONE',  ( -2.500000000000000888, 28.21753006952333109, -0.3272492347489316944 ) ) ;
#11461 = CARTESIAN_POINT ( 'NONE',  ( 0.8968807111111073427, 30.45845794433010312, 1.964841723554275221 ) ) ;
#11462 = ORIENTED_EDGE ( 'NONE', *, *, #6761, .T. ) ;
#11463 = CARTESIAN_POINT ( 'NONE',  ( 18.43520447300999976, -8.716575242777999222, 4.343080581981999977 ) ) ;
#11464 = CARTESIAN_POINT ( 'NONE',  ( 4.108142509193211112, 13.36663345100772382, -5.448696863470299689 ) ) ;
#11465 = CONICAL_SURFACE ( 'NONE', #21532, 4.649999926447000220, 0.7853981633972997312 ) ;
#11466 = DIRECTION ( 'NONE',  ( 0.000000000000000000, 1.000000000000000000, 0.000000000000000000 ) ) ;
#11467 = CIRCLE ( 'NONE', #11082, 2.948682383037074750 ) ;
#11468 = CARTESIAN_POINT ( 'NONE',  ( -22.67927891715234523, -7.913208109210116525, -6.993918658383377007 ) ) ;
#11469 = CYLINDRICAL_SURFACE ( 'NONE', #14666, 2.000000000000000000 ) ;
#11470 = B_SPLINE_CURVE_WITH_KNOTS ( 'NONE', 3,
 ( #7242, #7362, #7016, #21797, #14404, #23485, #12594, #21910, #16565, #6896, #18282, #5212, #14747, #8962, #19980, #1801, #1681, #20326, #22142, #5551, #14291, #10783, #18389, #22031, #16330, #12825, #21684, #14632, #5322, #23721, #9188, #7128, #12477, #12711, #19862, #10660, #20105, #12930, #11005, #3515, #16443, #9071, #5442, #20216, #3622, #20682, #5664, #15092, #6138, #13527, #20560, #9776, #4212, #11250, #20925, #18628 ),
 .UNSPECIFIED., .F., .F.,
 ( 4, 1, 1, 2, 2, 1, 1, 1, 1, 1, 2, 2, 1, 1, 1, 1, 1, 2, 2, 1, 1, 1, 1, 2, 2, 2, 2, 1, 2, 2, 1, 1, 1, 2, 2, 2, 2, 4 ),
 ( 0.000000000000000000, 0.06250000000000063838, 0.09375000000000109635, 0.1093750000000013323, 0.1250000000000015543, 0.1875000000000023870, 0.2187500000000027478, 0.2343750000000028588, 0.2421875000000028588, 0.2460937500000029421, 0.2480468750000029421, 0.2500000000000029976, 0.3125000000000032196, 0.3437500000000032196, 0.3593750000000032752, 0.3671875000000032752, 0.3710937500000032752, 0.3730468750000033307, 0.3750000000000033307, 0.4375000000000032196, 0.4687500000000032196, 0.4843750000000032752, 0.4921875000000033307, 0.4960937500000032752, 0.5000000000000032196, 0.5312500000000033307, 0.5625000000000033307, 0.5937500000000033307, 0.6093750000000033307, 0.6250000000000033307, 0.6875000000000034417, 0.7187500000000035527, 0.7343750000000036637, 0.7421875000000035527, 0.7500000000000035527, 0.8125000000000026645, 0.8750000000000016653, 1.000000000000000000 ),
 .UNSPECIFIED. ) ;
#11471 = ADVANCED_FACE ( 'NONE', ( #2545 ), #23561, .T. ) ;
#11472 = DIRECTION ( 'NONE',  ( 0.000000000000000000, 1.000000000000000000, 0.000000000000000000 ) ) ;
#11473 = ORIENTED_EDGE ( 'NONE', *, *, #5483, .F. ) ;
#11474 = CARTESIAN_POINT ( 'NONE',  ( -19.30321267869325652, -10.36687096048695089, 1.553511350694324777 ) ) ;
#11475 = CARTESIAN_POINT ( 'NONE',  ( 23.99062354302999722, -6.216878364870000340, -12.50000000000000000 ) ) ;
#11476 = AXIS2_PLACEMENT_3D ( 'NONE', #15667, #15552, #901 ) ;
#11477 = CARTESIAN_POINT ( 'NONE',  ( -1.861289502244705574, 28.35853889522002191, -1.170032434317527237 ) ) ;
#11478 = ORIENTED_EDGE ( 'NONE', *, *, #14977, .F. ) ;
#11479 = CARTESIAN_POINT ( 'NONE',  ( -23.74465998031000069, 13.93375672974000068, -0.8660254037843999608 ) ) ;
#11480 = AXIS2_PLACEMENT_3D ( 'NONE', #12570, #1555, #23699 ) ;
#11481 = CARTESIAN_POINT ( 'NONE',  ( 17.61412674930999955, -9.816082492500997958, -4.416083812485999793 ) ) ;
#11482 = EDGE_CURVE ( 'NONE', #21511, #21635, #19716, .T. ) ;
#11483 = CARTESIAN_POINT ( 'NONE',  ( -16.98505548173000079, 5.629683008772999209, -9.891015770318000833 ) ) ;
#11484 = DIRECTION ( 'NONE',  ( -1.000000000000000000, 0.000000000000000000, 0.000000000000000000 ) ) ;
#11485 = EDGE_CURVE ( 'NONE', #18033, #12379, #21651, .T. ) ;
#11486 = CARTESIAN_POINT ( 'NONE',  ( 13.22858580085999947, 9.111092516355000726, 6.665155751670000406 ) ) ;
#11487 = CARTESIAN_POINT ( 'NONE',  ( 0.3373768742556949585, 24.49999999999998224, 2.400465711495646914 ) ) ;
#11488 = CARTESIAN_POINT ( 'NONE',  ( 11.50000000000000000, 0.000000000000000000, 0.000000000000000000 ) ) ;
#11489 = CARTESIAN_POINT ( 'NONE',  ( 22.96884869472000190, 4.899556332588000274, 9.032014534518999938 ) ) ;
#11490 = CARTESIAN_POINT ( 'NONE',  ( 23.99999963380687618, 13.93375672974000246, -1.355252715606880543E-17 ) ) ;
#11491 = ORIENTED_EDGE ( 'NONE', *, *, #12823, .F. ) ;
#11492 = DIRECTION ( 'NONE',  ( -1.877655957117991099E-08, -0.9999999999999978906, 6.187284373139976848E-08 ) ) ;
#11493 = CARTESIAN_POINT ( 'NONE',  ( 0.05241653317063999645, 27.35706776952000041, 2.669209039122999894 ) ) ;
#11494 = CARTESIAN_POINT ( 'NONE',  ( 2.899213441999003216, 11.80143355452999110, 3.887780554085998652 ) ) ;
#11495 = AXIS2_PLACEMENT_3D ( 'NONE', #18412, #20237, #20581 ) ;
#11496 = CARTESIAN_POINT ( 'NONE',  ( 2.119314978498162638, 29.02854376302997252, -0.4166382853690258625 ) ) ;
#11497 = CARTESIAN_POINT ( 'NONE',  ( -21.60149277696999803, -3.745000288986999770, 10.44303877756999910 ) ) ;
#11498 = VERTEX_POINT ( 'NONE', #15130 ) ;
#11499 = EDGE_CURVE ( 'NONE', #16136, #8792, #11391, .T. ) ;
#11500 = EDGE_CURVE ( 'NONE', #9506, #3318, #1866, .T. ) ;
#11501 = CARTESIAN_POINT ( 'NONE',  ( -19.15130138363000611, -9.425786980393212389, 3.359030689042354911 ) ) ;
#11502 = VERTEX_POINT ( 'NONE', #18902 ) ;
#11503 = CARTESIAN_POINT ( 'NONE',  ( 15.71133103379665208, 7.256459353526666156, -5.576772732782599107 ) ) ;
#11504 = DIRECTION ( 'NONE',  ( 0.000000000000000000, 1.000000000000000000, 0.000000000000000000 ) ) ;
#11505 = CARTESIAN_POINT ( 'NONE',  ( 1.016344414748000080, 28.64506359724000362, 1.994688225595000253 ) ) ;
#11506 = CARTESIAN_POINT ( 'NONE',  ( -4.667964586162003826, 13.45633684249999895, 5.273208831630000759 ) ) ;
#11507 = CARTESIAN_POINT ( 'NONE',  ( 0.000000000000000000, -1.550000000000000044, 0.000000000000000000 ) ) ;
#11508 = CARTESIAN_POINT ( 'NONE',  ( 17.39475174931000012, -10.15246533026000186, 3.558175289345999914 ) ) ;
#11509 = CARTESIAN_POINT ( 'NONE',  ( -13.56430720021000091, -8.266217267278999969, 6.000601104121999541 ) ) ;
#11510 = CONICAL_SURFACE ( 'NONE', #12674, 9.630770167580999797, 0.9419447502231289571 ) ;
#11511 = CARTESIAN_POINT ( 'NONE',  ( -14.47793696890856019, 1.813149206526026624, 12.49999424749803012 ) ) ;
#11512 = ORIENTED_EDGE ( 'NONE', *, *, #10564, .F. ) ;
#11513 = CARTESIAN_POINT ( 'NONE',  ( -4.000000000000000000, 29.69999999999999929, 2.309401076759000304 ) ) ;
#11514 = CIRCLE ( 'NONE', #14964, 1.899912543625999373 ) ;
#11515 = CARTESIAN_POINT ( 'NONE',  ( -2.110727562395000145, 24.26086419343999978, 1.709321059049000002 ) ) ;
#11516 = CARTESIAN_POINT ( 'NONE',  ( 13.84581539899815539, -8.688513243712947087, 5.538713006654606197 ) ) ;
#11517 = CARTESIAN_POINT ( 'NONE',  ( 1.945894728673998708, 12.88054714962999903, -6.188039593268000793 ) ) ;
#11518 = CARTESIAN_POINT ( 'NONE',  ( 2.488228344306999684, 28.65086554002000341, 0.5718697359529000268 ) ) ;
#11519 = CARTESIAN_POINT ( 'NONE',  ( 11.40904387244352414, 2.948332260696533869, 12.49995270680734016 ) ) ;
#11520 = LINE ( 'NONE', #9695, #22749 ) ;
#11521 = FACE_OUTER_BOUND ( 'NONE', #21649, .T. ) ;
#11522 = DIRECTION ( 'NONE',  ( 0.000000000000000000, 1.000000000000000000, 0.000000000000000000 ) ) ;
#11523 = ORIENTED_EDGE ( 'NONE', *, *, #21982, .T. ) ;
#11524 = B_SPLINE_CURVE_WITH_KNOTS ( 'NONE', 3,
 ( #1295, #8683, #16050, #23443, #17645, #6620, #4813, #21647, #19588, #8318, #22214, #5408, #9276, #12895, #12676, #16294, #16531, #1767, #23687, #23918, #20294, #5629, #11217, #18596, #5748, #9154, #18246, #7329, #20532, #2001, #3698, #22334 ),
 .UNSPECIFIED., .F., .F.,
 ( 4, 2, 2, 2, 2, 2, 2, 2, 2, 2, 2, 2, 2, 2, 2, 4 ),
 ( 0.000000000000000000, 0.1249999999999995004, 0.1874999999999991396, 0.2187499999999990286, 0.2499999999999988898, 0.3124999999999987788, 0.3437499999999987232, 0.3749999999999987232, 0.4999999999999988898, 0.5624999999999990008, 0.5937499999999990008, 0.6249999999999988898, 0.6874999999999990008, 0.7187499999999991118, 0.7499999999999992228, 1.000000000000000000 ),
 .UNSPECIFIED. ) ;
#11525 = CARTESIAN_POINT ( 'NONE',  ( -4.000000000000000000, 28.30000000000000071, 2.309401076759000304 ) ) ;
#11526 = CIRCLE ( 'NONE', #11909, 3.000000000000000000 ) ;
#11527 = VERTEX_POINT ( 'NONE', #22763 ) ;
#11528 = B_SPLINE_SURFACE_WITH_KNOTS ( 'NONE', 3, 3, ( 
 ( #19250, #7869, #13429, #20830, #9924, #7988, #2662, #4356, #711, #4244, #15604, #6169, #11633, #19002, #6408, #2413, #15360, #13553, #20590, #20950, #6772, #16213, #12238, #5094, #8599, #15961, #23354, #956, #19379, #12360, #18046, #19625, #4975, #14165, #21560 ),
 ( #19748, #4606, #17561, #13790, #3159, #11994, #10541, #2789, #21682, #8354, #15846, #23235, #3033, #15719, #10174, #23111, #6649, #6535, #10421, #13919, #23610, #10658, #1207, #4850, #21315, #17926, #14044, #17812, #3275, #1331, #8720, #1451, #4729, #16084, #23483 ),
 ( #1082, #8847, #12116, #21192, #10294, #19502, #6894, #17682, #2911, #8481, #14289, #21437, #12475, #19860, #7125, #23719, #22029, #7360, #5440, #14857, #2033, #7473, #88, #12822, #16680, #5549, #22246, #19978, #20214, #1575, #22139, #23954, #12928, #20103, #3620 ),
 ( #14515, #13047, #12709, #20324, #18280, #3732, #9423, #14745, #18173, #3398, #5662, #16327, #21908, #20444, #11122, #5320, #10894, #11002, #18387, #3513, #18507, #1679, #9068, #3856, #1918, #11248, #10781, #18626, #16441, #16794, #8960, #7014, #23830, #7240, #14630 ) ),
 .UNSPECIFIED., .F., .F., .F.,
 ( 4, 4 ),
 ( 4, 1, 1, 1, 1, 1, 1, 1, 1, 1, 1, 1, 1, 1, 1, 1, 1, 1, 1, 1, 1, 1, 1, 1, 1, 1, 1, 1, 1, 1, 1, 1, 4 ),
 ( -0.3056682515952000023, 1.305668251594999996 ),
 ( 0.3076583088816999823, 0.3297182157065000063, 0.3517781225314000060, 0.3738380293562000301, 0.3958979361811000297, 0.4179578430058999983, 0.4400177498307999979, 0.4620776566556000220, 0.4841375634804999661, 0.5061974703053000457, 0.5282573771301999344, 0.5503172839550000139, 0.5723771907799000136, 0.5944370976046999822, 0.6164970044295999818, 0.6385569112543999504, 0.6606168180793000611, 0.6826767249041000296, 0.7047366317289999182, 0.7267965385537999978, 0.7488564453786000774, 0.7709163522034999660, 0.7929762590283000456, 0.8150361658531999343, 0.8370960726780000138, 0.8591559795029000135, 0.8812158863276999821, 0.9032757931526000927, 0.9253356999774000613, 0.9473956068022999499, 0.9694555136271000295, 0.9915154204520000292, 1.013575327277000060 ),
 .UNSPECIFIED. ) ;
#11529 = CARTESIAN_POINT ( 'NONE',  ( -5.776078224282449547, 16.26189775706639296, -2.037803783458385976 ) ) ;
#11530 = DIRECTION ( 'NONE',  ( 1.000000000000000000, 0.000000000000000000, 0.000000000000000000 ) ) ;
#11531 = CARTESIAN_POINT ( 'NONE',  ( 24.00016455292000117, -9.066063387507998783, 2.014468017461000127 ) ) ;
#11532 = VERTEX_POINT ( 'NONE', #7881 ) ;
#11533 = CARTESIAN_POINT ( 'NONE',  ( 14.47883169068999898, 6.653640265524000341, -8.778428370972001460 ) ) ;
#11534 = LINE ( 'NONE', #5944, #11760 ) ;
#11535 = CARTESIAN_POINT ( 'NONE',  ( 1.569224139466999901, 27.75962896667000024, 2.159851832628000068 ) ) ;
#11536 = ORIENTED_EDGE ( 'NONE', *, *, #3228, .F. ) ;
#11537 = ORIENTED_EDGE ( 'NONE', *, *, #7257, .F. ) ;
#11538 = CARTESIAN_POINT ( 'NONE',  ( -13.99999999999999645, 4.681959665041976137, -7.960623106173056129 ) ) ;
#11539 = CARTESIAN_POINT ( 'NONE',  ( -12.12711221169000098, 14.73199291194999994, 5.035616313343000527 ) ) ;
#11540 = CARTESIAN_POINT ( 'NONE',  ( 1.048658153906335100, 6.857636208004994849, -1.406037042848364838 ) ) ;
#11541 = CARTESIAN_POINT ( 'NONE',  ( 18.00945603379667048, 4.820354688224963269, 7.871655472196390946 ) ) ;
#11542 = ORIENTED_EDGE ( 'NONE', *, *, #6119, .F. ) ;
#11543 = CARTESIAN_POINT ( 'NONE',  ( -19.25994536489000097, 6.759255884526000457, 6.826644144461000430 ) ) ;
#11544 = CARTESIAN_POINT ( 'NONE',  ( -14.32799102833068616, 13.40593186268490911, 1.779780195171070334 ) ) ;
#11545 = CARTESIAN_POINT ( 'NONE',  ( 6.149053220390451102, 14.13825405241221667, 0.2391353124664657992 ) ) ;
#11546 = CARTESIAN_POINT ( 'NONE',  ( 15.41201067498107058, -1.444056539591619837, 10.25200677523064208 ) ) ;
#11547 = AXIS2_PLACEMENT_3D ( 'NONE', #16373, #10936, #18214 ) ;
#11548 = CARTESIAN_POINT ( 'NONE',  ( -15.70284115285000226, -10.90955963878999846, 1.677826734307000134 ) ) ;
#11549 = CARTESIAN_POINT ( 'NONE',  ( 0.2170015115553000085, 29.22007215129999835, -2.177509141144999827 ) ) ;
#11550 = CARTESIAN_POINT ( 'NONE',  ( -17.26141154489999963, -10.85036612823000013, 0.2443279951607999767 ) ) ;
#11551 = AXIS2_PLACEMENT_3D ( 'NONE', #7023, #1807, #18396 ) ;
#11552 = CARTESIAN_POINT ( 'NONE',  ( 0.005795789622999577249, 29.60418495093035673, 2.160003967929674751 ) ) ;
#11553 = ORIENTED_EDGE ( 'NONE', *, *, #15001, .T. ) ;
#11554 = CARTESIAN_POINT ( 'NONE',  ( 1.815810164558999906, 24.86381916441000328, -1.216941248911999951 ) ) ;
#11555 = AXIS2_PLACEMENT_3D ( 'NONE', #6227, #650, #2596 ) ;
#11556 = CARTESIAN_POINT ( 'NONE',  ( 0.000000000000000000, 7.000000000000000000, 0.000000000000000000 ) ) ;
#11557 = EDGE_LOOP ( 'NONE', ( #21607, #14567, #10499, #16674 ) ) ;
#11558 = DIRECTION ( 'NONE',  ( 1.000000000000000000, 0.000000000000000000, 0.000000000000000000 ) ) ;
#11559 = CARTESIAN_POINT ( 'NONE',  ( 0.000000000000000000, 28.30000000000000071, 0.000000000000000000 ) ) ;
#11560 = VECTOR ( 'NONE', #6214, 1000.000000000000000 ) ;
#11561 = CARTESIAN_POINT ( 'NONE',  ( -3.050000000000000266, 18.50000000000000000, 0.000000000000000000 ) ) ;
#11562 = EDGE_CURVE ( 'NONE', #9013, #611, #15249, .T. ) ;
#11563 = CARTESIAN_POINT ( 'NONE',  ( 16.92956408530999823, -4.671063266616000575, 9.108730853067999789 ) ) ;
#11564 = ORIENTED_EDGE ( 'NONE', *, *, #6458, .F. ) ;
#11565 = DIRECTION ( 'NONE',  ( 0.000000000000000000, -1.000000000000000000, 0.000000000000000000 ) ) ;
#11566 = CARTESIAN_POINT ( 'NONE',  ( 0.000000000000000000, 20.05000017415440183, 0.000000000000000000 ) ) ;
#11567 = VECTOR ( 'NONE', #14401, 1000.000000000000000 ) ;
#11568 = VERTEX_POINT ( 'NONE', #15372 ) ;
#11569 = CARTESIAN_POINT ( 'NONE',  ( -0.7783053373570000266, 84.95442836047000412, 5.000000000000000000 ) ) ;
#11570 = CYLINDRICAL_SURFACE ( 'NONE', #17086, 1.000000000000000222 ) ;
#11571 = CARTESIAN_POINT ( 'NONE',  ( 4.773276884097002792, 12.62757401777001931, 0.6733110646873000649 ) ) ;
#11572 = DIRECTION ( 'NONE',  ( 1.000000000000000000, 0.000000000000000000, 0.000000000000000000 ) ) ;
#11573 = AXIS2_PLACEMENT_3D ( 'NONE', #17782, #1301, #8692 ) ;
#11574 = CARTESIAN_POINT ( 'NONE',  ( -23.90296024929000041, -9.416283900593001022, 2.173132011546999642 ) ) ;
#11575 = EDGE_CURVE ( 'NONE', #1524, #8826, #7061, .T. ) ;
#11576 = CARTESIAN_POINT ( 'NONE',  ( -18.13088126894000141, 1.446686056264999920E-14, 0.000000000000000000 ) ) ;
#11577 = DIRECTION ( 'NONE',  ( -1.000000000000000000, 0.000000000000000000, 0.000000000000000000 ) ) ;
#11578 = FACE_BOUND ( 'NONE', #3273, .T. ) ;
#11579 = CARTESIAN_POINT ( 'NONE',  ( 1.259047450927247569, 28.76753006952334246, -2.184465970885645536 ) ) ;
#11580 = CARTESIAN_POINT ( 'NONE',  ( 2.500000000000000000, 27.85086340285666395, -0.3272492347489373565 ) ) ;
#11581 = CARTESIAN_POINT ( 'NONE',  ( 2.147225282976996219, 30.61754596991750077, -0.2336052812872324580 ) ) ;
#11582 = VERTEX_POINT ( 'NONE', #17825 ) ;
#11583 = CARTESIAN_POINT ( 'NONE',  ( -16.67449577250666692, -7.950790078334936339, 4.582403546340589884 ) ) ;
#11584 = CARTESIAN_POINT ( 'NONE',  ( 23.45972874556000320, 3.270437186057999934, 9.320145978262999620 ) ) ;
#11585 = CARTESIAN_POINT ( 'NONE',  ( -2.450733744771928624, 13.00631661139677497, -6.259151892297924569 ) ) ;
#11586 = CARTESIAN_POINT ( 'NONE',  ( 4.000000000000000000, 24.50000000000000000, 0.000000000000000000 ) ) ;
#11587 = AXIS2_PLACEMENT_3D ( 'NONE', #22829, #20788, #2373 ) ;
#11588 = CARTESIAN_POINT ( 'NONE',  ( 1.447934651311999943, 27.90196440325999916, 1.992911166421000191 ) ) ;
#11589 = CIRCLE ( 'NONE', #12384, 7.142857142857000241 ) ;
#11590 = B_SPLINE_CURVE_WITH_KNOTS ( 'NONE', 3,
 ( #10842, #16860, #18226, #1627, #20159 ),
 .UNSPECIFIED., .F., .F.,
 ( 4, 1, 4 ),
 ( 0.000000000000000000, 0.5000000000000000000, 1.000000000000000000 ),
 .UNSPECIFIED. ) ;
#11591 = AXIS2_PLACEMENT_3D ( 'NONE', #8523, #12629, #2946 ) ;
#11592 = DIRECTION ( 'NONE',  ( 0.000000000000000000, 1.000000000000000000, 0.000000000000000000 ) ) ;
#11593 = ORIENTED_EDGE ( 'NONE', *, *, #196, .T. ) ;
#11594 = EDGE_CURVE ( 'NONE', #9699, #4168, #9263, .T. ) ;
#11595 = CARTESIAN_POINT ( 'NONE',  ( -18.24258566398615500, 9.822636663924470213, 3.986703905974770201 ) ) ;
#11596 = DIRECTION ( 'NONE',  ( -1.000000000000000000, 0.000000000000000000, 0.000000000000000000 ) ) ;
#11597 = CARTESIAN_POINT ( 'NONE',  ( -1.433323533133572081, 28.32155547661488626, -1.629608261536916070 ) ) ;
#11598 = VERTEX_POINT ( 'NONE', #2924 ) ;
#11599 = EDGE_LOOP ( 'NONE', ( #23003, #12665, #21680, #13826, #3806 ) ) ;
#11600 = DIRECTION ( 'NONE',  ( -1.000000000000000000, 0.000000000000000000, 0.000000000000000000 ) ) ;
#11601 = CARTESIAN_POINT ( 'NONE',  ( 13.77506424931000240, -10.16002631551000057, 3.235559929811000046 ) ) ;
#11602 = EDGE_CURVE ( 'NONE', #13414, #5364, #12741, .T. ) ;
#11603 = CARTESIAN_POINT ( 'NONE',  ( 11.01624327026000039, 12.44999999999999929, 0.000000000000000000 ) ) ;
#11604 = FACE_BOUND ( 'NONE', #17494, .T. ) ;
#11605 = CARTESIAN_POINT ( 'NONE',  ( 13.29676537305999950, 10.72359741199000105, -0.7733205501537999682 ) ) ;
#11606 = CARTESIAN_POINT ( 'NONE',  ( -2.116994795175099142, 30.88300524173097017, -0.1245676364603316710 ) ) ;
#11607 = CARTESIAN_POINT ( 'NONE',  ( 8.124934037954998800, 1.125145054518999965E-14, 0.000000000000000000 ) ) ;
#11608 = CARTESIAN_POINT ( 'NONE',  ( 21.72950497963999794, -10.21084190113000112, 0.7917905117385000135 ) ) ;
#11609 = CARTESIAN_POINT ( 'NONE',  ( -2.999999956181000016, 17.90000004382000043, 2.609181505839000138E-08 ) ) ;
#11610 = ORIENTED_EDGE ( 'NONE', *, *, #17121, .T. ) ;
#11611 = CARTESIAN_POINT ( 'NONE',  ( 12.38482062235000036, -2.667901244413000139, -8.947351465620000610 ) ) ;
#11612 = CARTESIAN_POINT ( 'NONE',  ( 2.320116128650000054, 26.00000240009999786, 1.182158213329999930 ) ) ;
#11613 = VECTOR ( 'NONE', #18605, 1000.000000000000114 ) ;
#11614 = CARTESIAN_POINT ( 'NONE',  ( 4.258622327748002867, 12.20824998909998804, 2.305144079472002616 ) ) ;
#11615 = EDGE_CURVE ( 'NONE', #10557, #20433, #14843, .T. ) ;
#11616 = CARTESIAN_POINT ( 'NONE',  ( 2.154679880121377344, 28.99501662734741458, 0.1501254452029534836 ) ) ;
#11617 = CARTESIAN_POINT ( 'NONE',  ( -24.77609914680000358, -9.954456274527998971, -3.564765137135000206 ) ) ;
#11618 = ORIENTED_EDGE ( 'NONE', *, *, #2604, .T. ) ;
#11619 = CARTESIAN_POINT ( 'NONE',  ( 11.00000000000000000, 0.000000000000000000, 0.000000000000000000 ) ) ;
#11620 = VERTEX_POINT ( 'NONE', #1466 ) ;
#11621 = FACE_OUTER_BOUND ( 'NONE', #15629, .T. ) ;
#11622 = EDGE_CURVE ( 'NONE', #13433, #1329, #11206, .T. ) ;
#11623 = DIRECTION ( 'NONE',  ( 0.000000000000000000, -1.000000000000000000, 0.000000000000000000 ) ) ;
#11624 = CARTESIAN_POINT ( 'NONE',  ( -2.153772461420000006, 28.45006359724000333, 1.206163983883000057 ) ) ;
#11625 = EDGE_CURVE ( 'NONE', #6758, #1877, #8495, .T. ) ;
#11626 = CARTESIAN_POINT ( 'NONE',  ( 0.000000000000000000, 24.50000000000000000, 0.000000000000000000 ) ) ;
#11627 = CARTESIAN_POINT ( 'NONE',  ( 14.43318924931000069, 4.163528467249999920, -9.835102695514999382 ) ) ;
#11628 = CARTESIAN_POINT ( 'NONE',  ( -15.79874102787999846, 5.047191510808999304, 8.952058016012999886 ) ) ;
#11629 = CARTESIAN_POINT ( 'NONE',  ( 16.10887625731000128, 5.681759715831000257, 7.231772086132999711 ) ) ;
#11630 = CARTESIAN_POINT ( 'NONE',  ( -14.37382046149249071, 4.385283932934418871, 12.49975322910802511 ) ) ;
#11631 = ORIENTED_EDGE ( 'NONE', *, *, #17854, .F. ) ;
#11632 = ADVANCED_FACE ( 'NONE', ( #967 ), #10435, .T. ) ;
#11633 = CARTESIAN_POINT ( 'NONE',  ( -2.508635807456999434, 30.40905054822999887, -1.061151462325000017 ) ) ;
#11634 = EDGE_CURVE ( 'NONE', #10960, #1, #22018, .T. ) ;
#11635 = CARTESIAN_POINT ( 'NONE',  ( 1.234780954647000106, 24.81458662482000221, -2.203141158743999739 ) ) ;
#11636 = CARTESIAN_POINT ( 'NONE',  ( 14.19556169655588818, -8.215741800005648798, -6.232346285851887657 ) ) ;
#11637 = CARTESIAN_POINT ( 'NONE',  ( -4.353632028022997424, 13.53541229131999835, -4.749265782704001460 ) ) ;
#11638 = CARTESIAN_POINT ( 'NONE',  ( 20.16063042481999901, 5.004994577864000149, -10.01485155063000043 ) ) ;
#11639 = FACE_OUTER_BOUND ( 'NONE', #9666, .T. ) ;
#11640 = CARTESIAN_POINT ( 'NONE',  ( 11.39490977863705012, 2.886098606888460871, 12.49995748308370125 ) ) ;
#11641 = CARTESIAN_POINT ( 'NONE',  ( -1.963703823225463774, 26.25920717875808563, 0.8995588027868727243 ) ) ;
#11642 = LINE ( 'NONE', #7997, #2529 ) ;
#11643 = CARTESIAN_POINT ( 'NONE',  ( -6.250000012226999857, 15.73199627394999922, 1.185103398761000015 ) ) ;
#11644 = CARTESIAN_POINT ( 'NONE',  ( 2.500000000000000000, 24.63419673618999894, 0.000000000000000000 ) ) ;
#11645 = ORIENTED_EDGE ( 'NONE', *, *, #9965, .F. ) ;
#11646 = CARTESIAN_POINT ( 'NONE',  ( 0.9226519948152428485, 23.99124041189808310, -2.329934127714008429 ) ) ;
#11647 = B_SPLINE_CURVE_WITH_KNOTS ( 'NONE', 3,
 ( #8408, #19552, #8283, #19305, #15647, #21115, #1256, #21361 ),
 .UNSPECIFIED., .F., .F.,
 ( 4, 2, 2, 4 ),
 ( 0.000000000000000000, 0.2499999999999998890, 0.4999999999999997780, 1.000000000000000000 ),
 .UNSPECIFIED. ) ;
#11648 = ORIENTED_EDGE ( 'NONE', *, *, #1934, .T. ) ;
#11649 = CARTESIAN_POINT ( 'NONE',  ( -5.987337191874583908, 16.36486391838442955, -1.335248119225510566 ) ) ;
#11651 = CARTESIAN_POINT ( 'NONE',  ( -2.051578334272556425, 24.64979581979662626, 0.7778699027752854489 ) ) ;
#11650 = DIRECTION ( 'NONE',  ( 0.000000000000000000, 1.000000000000000000, 0.000000000000000000 ) ) ;
#11652 = DIRECTION ( 'NONE',  ( -1.000000000000000000, 0.000000000000000000, 0.000000000000000000 ) ) ;
#11653 = CARTESIAN_POINT ( 'NONE',  ( 6.143312206438239720, 14.17910314525702375, -0.1182593359610033257 ) ) ;
#11654 = CARTESIAN_POINT ( 'NONE',  ( -20.31751159899667769, -7.761064575021531020, 5.041909840973705315 ) ) ;
#11655 = LINE ( 'NONE', #19026, #20601 ) ;
#11656 = ORIENTED_EDGE ( 'NONE', *, *, #3772, .F. ) ;
#11657 = ORIENTED_EDGE ( 'NONE', *, *, #18219, .F. ) ;
#11658 = DIRECTION ( 'NONE',  ( -0.8181527231370768760, 0.000000000000000000, -0.5750009753238559673 ) ) ;
#11659 = CARTESIAN_POINT ( 'NONE',  ( -0.6619726575697483240, 6.809906748830050205, -1.620274423901518768 ) ) ;
#11660 = CYLINDRICAL_SURFACE ( 'NONE', #19482, 4.750000000000000000 ) ;
#11661 = ORIENTED_EDGE ( 'NONE', *, *, #10771, .T. ) ;
#11662 = ADVANCED_FACE ( 'NONE', ( #4862 ), #23497, .F. ) ;
#11663 = CARTESIAN_POINT ( 'NONE',  ( -22.58843503502000161, -9.116449256743999641, 4.620077567651999395 ) ) ;
#11664 = FACE_OUTER_BOUND ( 'NONE', #12971, .T. ) ;
#11665 = CARTESIAN_POINT ( 'NONE',  ( 6.157535982278581344, 14.08554119385395964, 0.3695686495852765208 ) ) ;
#11666 = CARTESIAN_POINT ( 'NONE',  ( 15.38005428219763893, -0.3122026486411542678, 10.35019470995840507 ) ) ;
#11667 = LINE ( 'NONE', #506, #22218 ) ;
#11668 = CARTESIAN_POINT ( 'NONE',  ( 1.574276030777000068, 30.48667273621999740, -1.526313238878999945 ) ) ;
#11669 = LINE ( 'NONE', #10461, #2689 ) ;
#11670 = CARTESIAN_POINT ( 'NONE',  ( -13.76743754818000021, -2.422432655768999687, 9.928996171009998761 ) ) ;
#11671 = CARTESIAN_POINT ( 'NONE',  ( 0.5301375200171086766, 29.63531083614599737, 2.093953783698239590 ) ) ;
#11672 = ORIENTED_EDGE ( 'NONE', *, *, #10987, .F. ) ;
#11673 = B_SPLINE_CURVE_WITH_KNOTS ( 'NONE', 3,
 ( #11886, #6187, #19270, #2684, #10072, #17457, #850, #8255, #4995, #5227 ),
 .UNSPECIFIED., .F., .F.,
 ( 4, 2, 2, 2, 4 ),
 ( 0.000000000000000000, 0.2499999999999998890, 0.4999999999999997780, 0.7499999999999998890, 1.000000000000000000 ),
 .UNSPECIFIED. ) ;
#11674 = CARTESIAN_POINT ( 'NONE',  ( -0.2719153812508000034, 25.03673698483999743, -2.333095969081999677 ) ) ;
#11675 = CARTESIAN_POINT ( 'NONE',  ( 18.22028936713000036, -1.652712406954000013, 8.988165862088999702 ) ) ;
#11676 = VERTEX_POINT ( 'NONE', #7027 ) ;
#11677 = CARTESIAN_POINT ( 'NONE',  ( -2.241935917934180011, 24.64274320532739893, -0.3031776926340762901 ) ) ;
#11678 = CARTESIAN_POINT ( 'NONE',  ( -5.147424556882004509, 15.83079896314000301, 2.717927425388003027 ) ) ;
#11679 = CARTESIAN_POINT ( 'NONE',  ( -9.000000000000000000, 19.50000000000000000, -1.000000000000000000 ) ) ;
#11680 = CARTESIAN_POINT ( 'NONE',  ( 17.47800158530999681, -7.122204577229999778, -7.372745388647000020 ) ) ;
#11681 = ORIENTED_EDGE ( 'NONE', *, *, #1568, .T. ) ;
#11682 = CARTESIAN_POINT ( 'NONE',  ( -6.116766749681998405, 16.13602277433998466, -0.9718497405647000820 ) ) ;
#11683 = CARTESIAN_POINT ( 'NONE',  ( 24.34804274388857337, -12.49056186101158872, 3.365712241645715253 ) ) ;
#11684 = VECTOR ( 'NONE', #8929, 1000.000000000000000 ) ;
#11685 = ORIENTED_EDGE ( 'NONE', *, *, #10475, .F. ) ;
#11686 = DIRECTION ( 'NONE',  ( 0.000000000000000000, 0.000000000000000000, -1.000000000000000000 ) ) ;
#11687 = DIRECTION ( 'NONE',  ( 0.000000000000000000, 1.000000000000000000, 0.000000000000000000 ) ) ;
#11688 = CARTESIAN_POINT ( 'NONE',  ( -4.811457632815001162, 12.64231287075998900, -0.1525242827666000722 ) ) ;
#11689 = CARTESIAN_POINT ( 'NONE',  ( 18.93264468355999952, 0.000000000000000000, 0.000000000000000000 ) ) ;
#11690 = CARTESIAN_POINT ( 'NONE',  ( 17.77671462316595807, -9.250044903823519959, -4.891976846289935565 ) ) ;
#11691 = CARTESIAN_POINT ( 'NONE',  ( -2.121106334292000017, 30.87889366360999688, 6.284935476095000148E-07 ) ) ;
#11692 = LINE ( 'NONE', #20651, #23826 ) ;
#11693 = CARTESIAN_POINT ( 'NONE',  ( -4.820913537080000033, 13.20111002679000123, 5.836439296936000609 ) ) ;
#11694 = CARTESIAN_POINT ( 'NONE',  ( -0.9358744650684699407, 26.41068681084919589, 4.078474779182607257 ) ) ;
#11695 =( NAMED_UNIT ( * ) PLANE_ANGLE_UNIT ( ) SI_UNIT ( $, .RADIAN. ) );
#11696 = LINE ( 'NONE', #18714, #12655 ) ;
#11697 = EDGE_CURVE ( 'NONE', #23530, #20521, #21212, .T. ) ;
#11698 = CARTESIAN_POINT ( 'NONE',  ( 0.6344839516865840023, 30.44182778481178175, 2.065287063757580199 ) ) ;
#11699 = EDGE_LOOP ( 'NONE', ( #15269, #19283, #5965 ) ) ;
#11700 = CARTESIAN_POINT ( 'NONE',  ( 23.84623061267999944, -8.327348115725000000, 5.332256611120000045 ) ) ;
#11701 = CARTESIAN_POINT ( 'NONE',  ( 2.743213193691274032, 13.05670274646432105, -6.153260231641096922 ) ) ;
#11702 = DIRECTION ( 'NONE',  ( 1.000000000000000000, 0.000000000000000000, 0.000000000000000000 ) ) ;
#11703 = CARTESIAN_POINT ( 'NONE',  ( 0.000000000000000000, 18.10000000000000142, 0.000000000000000000 ) ) ;
#11704 = CARTESIAN_POINT ( 'NONE',  ( -0.6219987658658999718, 25.85446440325999973, -2.383523424258999768 ) ) ;
#11705 = B_SPLINE_CURVE_WITH_KNOTS ( 'NONE', 3,
 ( #22380, #22969, #2641, #10036 ),
 .UNSPECIFIED., .F., .F.,
 ( 4, 4 ),
 ( 0.000000000000000000, 1.000000000000000000 ),
 .UNSPECIFIED. ) ;
#11706 = AXIS2_PLACEMENT_3D ( 'NONE', #21617, #5033, #12985 ) ;
#11707 = CARTESIAN_POINT ( 'NONE',  ( -10.04701370329000021, 16.31160201364000173, 0.9999999999983000265 ) ) ;
#11708 = ORIENTED_EDGE ( 'NONE', *, *, #4022, .F. ) ;
#11709 = CARTESIAN_POINT ( 'NONE',  ( -17.48898225880079238, -10.32045256900975971, 1.544200643038546872 ) ) ;
#11710 = EDGE_CURVE ( 'NONE', #2875, #9862, #22777, .T. ) ;
#11711 = LINE ( 'NONE', #21026, #16545 ) ;
#11712 = CARTESIAN_POINT ( 'NONE',  ( 0.000000000000000000, 24.65000000674550051, 0.000000000000000000 ) ) ;
#11713 = FACE_OUTER_BOUND ( 'NONE', #10863, .T. ) ;
#11714 = ORIENTED_EDGE ( 'NONE', *, *, #12377, .T. ) ;
#11715 = DIRECTION ( 'NONE',  ( 0.000000000000000000, 0.9145998131564575528, -0.4043602128970813503 ) ) ;
#11716 = CARTESIAN_POINT ( 'NONE',  ( 11.77425158531000093, -9.807789133420998340, 1.022826625653000088 ) ) ;
#11717 = PLANE ( 'NONE',  #13135 ) ;
#11718 = CARTESIAN_POINT ( 'NONE',  ( -10.04351714999000045, 16.35737901937999794, 1.000000000001999956 ) ) ;
#11719 = CARTESIAN_POINT ( 'NONE',  ( 13.43171080085999947, 2.637024924671000470, 10.98238284665000108 ) ) ;
#11720 = DIRECTION ( 'NONE',  ( -1.576598371538795140E-18, -7.363899292998020299E-10, 1.000000000000000000 ) ) ;
#11721 = CIRCLE ( 'NONE', #9777, 2.649999999999999911 ) ;
#11722 = CARTESIAN_POINT ( 'NONE',  ( -5.625000000000000000, 21.50000000000000000, -1.676174921084000144E-09 ) ) ;
#11723 = CARTESIAN_POINT ( 'NONE',  ( 24.30244787985000343, 0.3995280882934000299, -9.774475514773000029 ) ) ;
#11724 = EDGE_CURVE ( 'NONE', #7720, #3069, #3036, .T. ) ;
#11725 = LINE ( 'NONE', #8096, #16194 ) ;
#11726 = ORIENTED_EDGE ( 'NONE', *, *, #8054, .F. ) ;
#11727 = LINE ( 'NONE', #19101, #22359 ) ;
#11728 = CARTESIAN_POINT ( 'NONE',  ( 2.157402177123000087, 25.89456776952000183, 1.099251314038999894 ) ) ;
#11729 = CARTESIAN_POINT ( 'NONE',  ( 4.150310933805998914, 12.32001967052000424, 2.267141452629003240 ) ) ;
#11730 = CARTESIAN_POINT ( 'NONE',  ( 2.098996325922923845, 29.03416195166998293, -0.5104432153915662296 ) ) ;
#11731 = CARTESIAN_POINT ( 'NONE',  ( -22.10274641431000120, 10.93051552941000004, 1.976840160283999781 ) ) ;
#11732 = ORIENTED_EDGE ( 'NONE', *, *, #18428, .F. ) ;
#11733 = CARTESIAN_POINT ( 'NONE',  ( -23.16929462096833703, 9.265295224643226746, 1.607743681355135241E-05 ) ) ;
#11734 = VERTEX_POINT ( 'NONE', #23731 ) ;
#11735 = DIRECTION ( 'NONE',  ( 1.000000000000000000, 0.000000000000000000, 0.000000000000000000 ) ) ;
#11736 = FACE_BOUND ( 'NONE', #19907, .T. ) ;
#11737 = EDGE_CURVE ( 'NONE', #11953, #5391, #23967, .T. ) ;
#11738 = CARTESIAN_POINT ( 'NONE',  ( 5.043056616458001962, 13.80554412637000006, 4.028432506473001773 ) ) ;
#11739 = CARTESIAN_POINT ( 'NONE',  ( 1.065753921018558481, 6.860530577516010808, 1.391907256200018761 ) ) ;
#11740 = CARTESIAN_POINT ( 'NONE',  ( 12.78787674931000140, 8.861872729009999006, -5.882981327196000088 ) ) ;
#11741 = AXIS2_PLACEMENT_3D ( 'NONE', #16758, #21877, #14598 ) ;
#11742 = CARTESIAN_POINT ( 'NONE',  ( -18.88645432865000018, -8.793774626762999702, -6.438463651166999924 ) ) ;
#11743 = CARTESIAN_POINT ( 'NONE',  ( 11.83106375730999993, 2.025755645688000151, -8.855592440447001223 ) ) ;
#11744 = ADVANCED_FACE ( 'NONE', ( #10793 ), #18544, .T. ) ;
#11745 = DIRECTION ( 'NONE',  ( -1.000000000000000000, 0.000000000000000000, 0.000000000000000000 ) ) ;
#11746 = VERTEX_POINT ( 'NONE', #3524 ) ;
#11747 = CARTESIAN_POINT ( 'NONE',  ( -4.000000000000000888, 29.87490599056224383, 1.464369514602714251 ) ) ;
#11748 = B_SPLINE_CURVE_WITH_KNOTS ( 'NONE', 3,
 ( #3317, #23650, #12403, #5247, #16605, #10698, #5018, #16257 ),
 .UNSPECIFIED., .F., .F.,
 ( 4, 2, 2, 4 ),
 ( 2.284496667305657708E-05, 0.0004791365171912424304, 0.0009354280677094282091, 0.001848011168745799983 ),
 .UNSPECIFIED. ) ;
#11749 = CARTESIAN_POINT ( 'NONE',  ( -1.513605150068000116, 23.59780545119999928, 2.021779747291999829 ) ) ;
#11750 = CARTESIAN_POINT ( 'NONE',  ( 14.21171828542962423, -7.852796259521285016, -6.687517491369988853 ) ) ;
#11751 = APPLICATION_CONTEXT ( 'automotive_design' ) ;
#11752 = CARTESIAN_POINT ( 'NONE',  ( -3.787113239318998570, 13.89839096013999509, -4.743087660284001750 ) ) ;
#11753 = CARTESIAN_POINT ( 'NONE',  ( 19.12053096800999796, 0.006299968456938000866, 10.67181407054999909 ) ) ;
#11754 = EDGE_CURVE ( 'NONE', #6219, #20600, #13500, .T. ) ;
#11755 = CARTESIAN_POINT ( 'NONE',  ( 2.000000000000000000, 26.50000000000000355, 3.464101615137999968 ) ) ;
#11756 = CARTESIAN_POINT ( 'NONE',  ( 11.22311500623200153, 2.002057944010465107, 12.49998975379359756 ) ) ;
#11757 = CARTESIAN_POINT ( 'NONE',  ( 18.07193721978578793, 6.079758669371162050, -8.513683897598470551 ) ) ;
#11758 = DIRECTION ( 'NONE',  ( 0.000000000000000000, -1.000000000000000000, 0.000000000000000000 ) ) ;
#11759 = CARTESIAN_POINT ( 'NONE',  ( -21.54962077250665686, -1.207329456531916589, -9.224287454130459807 ) ) ;
#11760 = VECTOR ( 'NONE', #11056, 1000.000000000000000 ) ;
#11761 = CARTESIAN_POINT ( 'NONE',  ( 24.50000000000000711, -11.08150693382694030, -5.806266966183555311 ) ) ;
#11762 = ORIENTED_EDGE ( 'NONE', *, *, #10098, .F. ) ;
#11763 = CARTESIAN_POINT ( 'NONE',  ( 11.31235608933860526, -12.07787442533556899, 4.080443649533860295 ) ) ;
#11764 = EDGE_LOOP ( 'NONE', ( #12604, #373, #1205 ) ) ;
#11765 = CARTESIAN_POINT ( 'NONE',  ( -5.902050209366081823, 16.32236802668609243, -1.677094527035041693 ) ) ;
#11767 = CARTESIAN_POINT ( 'NONE',  ( -2.148333256768187205, 23.64833325676920595, 0.1693336218410599059 ) ) ;
#11766 = DIRECTION ( 'NONE',  ( 0.000000000000000000, 0.9998336578527885488, 0.01823887673933978840 ) ) ;
#11768 = EDGE_CURVE ( 'NONE', #10482, #4536, #1578, .T. ) ;
#11769 = DIRECTION ( 'NONE',  ( 0.000000000000000000, 0.000000000000000000, -1.000000000000000000 ) ) ;
#11770 = TOROIDAL_SURFACE ( 'NONE', #7500, 1.600000000000000089, 0.1000000000000000056 ) ;
#11771 = DIRECTION ( 'NONE',  ( -1.000000000000000000, 0.000000000000000000, 0.000000000000000000 ) ) ;
#11772 = CARTESIAN_POINT ( 'NONE',  ( -21.05832910583999862, 9.211679941677999750, 0.000000000000000000 ) ) ;
#11773 = CARTESIAN_POINT ( 'NONE',  ( 17.71428936713000013, 9.125865291226999076, 0.000000000000000000 ) ) ;
#11774 = EDGE_LOOP ( 'NONE', ( #4637, #7517, #11424, #15325 ) ) ;
#11775 = VERTEX_POINT ( 'NONE', #14527 ) ;
#11776 = CARTESIAN_POINT ( 'NONE',  ( -14.00000000000000000, -4.254780838336652771, -8.767722819108374921 ) ) ;
#11777 = CARTESIAN_POINT ( 'NONE',  ( 2.693005968609320178, 29.96241504948189416, -3.063994432611676366 ) ) ;
#11778 = CARTESIAN_POINT ( 'NONE',  ( -24.50000000000000000, -10.82531754731000007, -6.250000000000000000 ) ) ;
#11779 = VERTEX_POINT ( 'NONE', #19990 ) ;
#11780 = CARTESIAN_POINT ( 'NONE',  ( -20.28814577853999523, -8.980834437001998793, -3.489049909224000157 ) ) ;
#11781 = LINE ( 'NONE', #13704, #7843 ) ;
#11782 = DIRECTION ( 'NONE',  ( 1.000000000000000000, 0.000000000000000000, 0.000000000000000000 ) ) ;
#11783 = CARTESIAN_POINT ( 'NONE',  ( 15.87393906135570276, -10.20432133770710159, -1.800441640727369563 ) ) ;
#11784 = CARTESIAN_POINT ( 'NONE',  ( -16.57211600987000111, 9.781171088540000724, 5.166091611002999961 ) ) ;
#11785 = ADVANCED_FACE ( 'NONE', ( #22042 ), #18919, .T. ) ;
#11786 = CARTESIAN_POINT ( 'NONE',  ( 1.575836833087000066, 29.72868779823999930, -1.751713004377999816 ) ) ;
#11787 = CARTESIAN_POINT ( 'NONE',  ( -20.38137539109145280, 10.48768805034149487, -0.5609562679966193510 ) ) ;
#11788 = ADVANCED_FACE ( 'NONE', ( #22153 ), #18475, .F. ) ;
#11789 = CARTESIAN_POINT ( 'NONE',  ( 0.000000000000000000, 14.90000000000000036, 0.000000000000000000 ) ) ;
#11790 = CARTESIAN_POINT ( 'NONE',  ( -1.099324150219182838, 29.53577431558094446, 1.859157437254163714 ) ) ;
#11791 = VERTEX_POINT ( 'NONE', #11979 ) ;
#11792 = CIRCLE ( 'NONE', #14487, 4.750000000000000000 ) ;
#11793 = CARTESIAN_POINT ( 'NONE',  ( -18.28298561839290670, 6.265330369647709396, 8.380266679069755753 ) ) ;
#11794 = ORIENTED_EDGE ( 'NONE', *, *, #7921, .F. ) ;
#11795 = CARTESIAN_POINT ( 'NONE',  ( 5.325462603570996656, 13.97134787008000067, -3.325730261421003142 ) ) ;
#11796 = ADVANCED_FACE ( 'NONE', ( #10643 ), #14787, .F. ) ;
#11797 = DIRECTION ( 'NONE',  ( 0.000000000000000000, 1.000000000000000000, 0.000000000000000000 ) ) ;
#11798 = CIRCLE ( 'NONE', #16968, 7.500000000000000000 ) ;
#11799 = CARTESIAN_POINT ( 'NONE',  ( 1.699986466736000068, 9.100024030970999434, -1.053574575520999757 ) ) ;
#11800 = CARTESIAN_POINT ( 'NONE',  ( 13.83187642131000139, 0.1979999634357000049, -9.644016179210000317 ) ) ;
#11801 = EDGE_LOOP ( 'NONE', ( #20036, #9883, #20318, #23205, #3110, #9115, #12767 ) ) ;
#11802 = PLANE ( 'NONE',  #7501 ) ;
#11803 = CARTESIAN_POINT ( 'NONE',  ( -0.3502059142650870704, 24.70197603011383691, -4.416610674644637413 ) ) ;
#11804 = CARTESIAN_POINT ( 'NONE',  ( 0.000000000000000000, 24.80000000000000426, 4.618802153517000519 ) ) ;
#11805 = VERTEX_POINT ( 'NONE', #8073 ) ;
#11806 = CARTESIAN_POINT ( 'NONE',  ( -1.219598243196123644, 24.73228032484876593, 1.802923274881913729 ) ) ;
#11807 = CARTESIAN_POINT ( 'NONE',  ( 11.49999999537000051, -6.999999995366000149, -1.987954085830999545E-09 ) ) ;
#11808 = CARTESIAN_POINT ( 'NONE',  ( 23.91181431106168631, 9.664920907709271702, 4.394489354301833295 ) ) ;
#11809 = VECTOR ( 'NONE', #13200, 1000.000000000000000 ) ;
#11810 = CARTESIAN_POINT ( 'NONE',  ( 4.000000000000000000, 26.43562577624026488, 1.040161751118762634 ) ) ;
#11811 = CARTESIAN_POINT ( 'NONE',  ( 17.66192372649435427, -10.35977045958544807, -0.9250195969887425873 ) ) ;
#11812 = CARTESIAN_POINT ( 'NONE',  ( 0.7867367962552690441, 24.50000000000000000, -2.267387309971103271 ) ) ;
#11813 = CARTESIAN_POINT ( 'NONE',  ( -14.45561362881484335, -9.532958125082343415, 8.488361093024359150 ) ) ;
#11814 = CARTESIAN_POINT ( 'NONE',  ( 24.43180435030999931, -9.516463450214999398, 5.130367153252000101 ) ) ;
#11815 = DIRECTION ( 'NONE',  ( 0.000000000000000000, 1.000000000000000000, 0.000000000000000000 ) ) ;
#11816 = CARTESIAN_POINT ( 'NONE',  ( -1.259047450927251788, 28.90086340285667532, -2.184465970885643316 ) ) ;
#11817 = CARTESIAN_POINT ( 'NONE',  ( 66.60588651278291650, 36.26856778792605240, 0.000000000000000000 ) ) ;
#11818 = CARTESIAN_POINT ( 'NONE',  ( -1.317397315007501346, 30.08744644730780493, -1.712080957474261478 ) ) ;
#11819 = ORIENTED_EDGE ( 'NONE', *, *, #18114, .F. ) ;
#11820 = CARTESIAN_POINT ( 'NONE',  ( 19.06751900412999845, -6.585038314783999702, -7.908837097906999958 ) ) ;
#11821 = CARTESIAN_POINT ( 'NONE',  ( 1.979184699210071896, 12.93672951579921815, -6.401123758412539999 ) ) ;
#11822 = CARTESIAN_POINT ( 'NONE',  ( 8.124934037954998800, -14.44999999999999929, 0.000000000000000000 ) ) ;
#11823 = CARTESIAN_POINT ( 'NONE',  ( -20.13552329019880460, 10.43394003992358599, 1.146997921864789882 ) ) ;
#11824 = DIRECTION ( 'NONE',  ( -8.117316429522999705E-13, 1.000000000000000000, -5.625591667474000414E-11 ) ) ;
#11825 = AXIS2_PLACEMENT_3D ( 'NONE', #12719, #23364, #23494 ) ;
#11826 = CARTESIAN_POINT ( 'NONE',  ( 0.000000000000000000, 28.30000000000000071, 4.618802153517000519 ) ) ;
#11827 = ORIENTED_EDGE ( 'NONE', *, *, #15224, .T. ) ;
#11828 = CARTESIAN_POINT ( 'NONE',  ( -17.62853844494577871, -8.423990400856537164, 6.160666632630097617 ) ) ;
#11829 = DIRECTION ( 'NONE',  ( -1.000000000000000000, 0.000000000000000000, 0.000000000000000000 ) ) ;
#11830 = CARTESIAN_POINT ( 'NONE',  ( 1.671483013463360923, 27.93939348436179060, 1.428772922976359050 ) ) ;
#11831 = DIRECTION ( 'NONE',  ( 1.000000000000000000, 0.000000000000000000, 0.000000000000000000 ) ) ;
#11832 = CARTESIAN_POINT ( 'NONE',  ( -14.25000000000000000, 0.000000000000000000, 0.000000000000000000 ) ) ;
#11833 = ADVANCED_FACE ( 'NONE', ( #22475 ), #11469, .T. ) ;
#11834 = ORIENTED_EDGE ( 'NONE', *, *, #15602, .F. ) ;
#11835 = CARTESIAN_POINT ( 'NONE',  ( 16.95845603379666855, -7.957157342237437092, -4.586073407758718190 ) ) ;
#11836 = CARTESIAN_POINT ( 'NONE',  ( 16.73662674931000183, 9.294473935295998857, 5.382749556855999984 ) ) ;
#11837 = CARTESIAN_POINT ( 'NONE',  ( -14.14777689704998487, 3.317162000593086635, -8.454068354355397830 ) ) ;
#11838 = CARTESIAN_POINT ( 'NONE',  ( 18.51344355829000321, -6.966878364870000340, 12.06698729810999993 ) ) ;
#11839 = FACE_OUTER_BOUND ( 'NONE', #11079, .T. ) ;
#11840 = CARTESIAN_POINT ( 'NONE',  ( 13.56806994526000132, 10.19277579189000171, -0.7351067978804000091 ) ) ;
#11841 = LINE ( 'NONE', #23330, #12408 ) ;
#11842 = AXIS2_PLACEMENT_3D ( 'NONE', #3579, #19820, #10962 ) ;
#11843 = B_SPLINE_CURVE_WITH_KNOTS ( 'NONE', 3,
 ( #20017, #3659, #8761, #8887, #12857, #16124, #7056, #14441, #18212, #6938, #17966, #14334, #19789, #23873, #3438, #1370, #20255, #16369 ),
 .UNSPECIFIED., .F., .F.,
 ( 4, 2, 2, 2, 2, 2, 2, 2, 4 ),
 ( 0.000000000000000000, 0.1250000000000000833, 0.2500000000000001665, 0.3750000000000002220, 0.5000000000000002220, 0.6250000000000002220, 0.7500000000000001110, 0.8750000000000001110, 1.000000000000000000 ),
 .UNSPECIFIED. ) ;
#11844 = CARTESIAN_POINT ( 'NONE',  ( -4.563746053395999702, 26.50000000000000000, 4.080056528100000079 ) ) ;
#11845 = CARTESIAN_POINT ( 'NONE',  ( 22.88605506260999789, 9.630491853314000039, -1.482563043280999970 ) ) ;
#11846 = CARTESIAN_POINT ( 'NONE',  ( 8.196152422706999729, 26.90192378864669820, 6.000000000000000000 ) ) ;
#11847 = EDGE_LOOP ( 'NONE', ( #12673, #4403, #2412, #10933 ) ) ;
#11848 = CARTESIAN_POINT ( 'NONE',  ( 2.374386521520468918, 13.96624173149727000, 5.647372986366287151 ) ) ;
#11849 = CARTESIAN_POINT ( 'NONE',  ( -2.656868203660999850, 27.94206776952000126, -0.2616786785207999566 ) ) ;
#11850 = CARTESIAN_POINT ( 'NONE',  ( -3.143058089422002599, 11.99907213748002022, 3.545075994667000518 ) ) ;
#11851 = CARTESIAN_POINT ( 'NONE',  ( 2.053969861739825653, 29.04388804318223194, -0.6701222371007186096 ) ) ;
#11852 = CARTESIAN_POINT ( 'NONE',  ( -22.26983096010000196, 10.23598255321000039, -4.325444529497999291 ) ) ;
#11853 = CARTESIAN_POINT ( 'NONE',  ( -2.500000000000000000, 28.00000000000000000, 0.000000000000000000 ) ) ;
#11854 = ORIENTED_EDGE ( 'NONE', *, *, #2389, .F. ) ;
#11855 = DIRECTION ( 'NONE',  ( -1.000000000000000000, 0.000000000000000000, 0.000000000000000000 ) ) ;
#11856 = CARTESIAN_POINT ( 'NONE',  ( 0.000000000000000000, 20.04999987253367877, 0.000000000000000000 ) ) ;
#11857 = VECTOR ( 'NONE', #6804, 1000.000000000000114 ) ;
#11858 = CARTESIAN_POINT ( 'NONE',  ( -1.734941855790413712, 6.996073985788684446, 0.2676728999513400820 ) ) ;
#11859 = CARTESIAN_POINT ( 'NONE',  ( -14.25243324638999809, 7.716878364870000340, 11.63397459621999985 ) ) ;
#11860 = ADVANCED_FACE ( 'NONE', ( #5999 ), #15815, .F. ) ;
#11861 = CARTESIAN_POINT ( 'NONE',  ( -16.61126241975999918, -1.906005702182999917, -10.12158796435999975 ) ) ;
#11862 = CARTESIAN_POINT ( 'NONE',  ( 16.65731375730999986, -8.692770150473998925, 3.046645682941000022 ) ) ;
#11863 = CARTESIAN_POINT ( 'NONE',  ( 18.93668626432143753, 2.220822707206575597, 10.19564009161587492 ) ) ;
#11864 = ORIENTED_EDGE ( 'NONE', *, *, #15398, .T. ) ;
#11865 = CARTESIAN_POINT ( 'NONE',  ( 21.19112270046331403, 8.051969607661357387, -4.641010349315714656 ) ) ;
#11866 =( NAMED_UNIT ( * ) SI_UNIT ( $, .STERADIAN. ) SOLID_ANGLE_UNIT ( ) );
#11867 = CIRCLE ( 'NONE', #630, 11.50000000000000000 ) ;
#11868 = CARTESIAN_POINT ( 'NONE',  ( -0.3563741520152000075, 25.15743979504999928, 2.692573825428000056 ) ) ;
#11869 = CARTESIAN_POINT ( 'NONE',  ( 3.240158297419062361, 14.20012988688566402, -5.197965063808845265 ) ) ;
#11870 = EDGE_LOOP ( 'NONE', ( #3031, #10177, #11661, #1057 ) ) ;
#11871 = AXIS2_PLACEMENT_3D ( 'NONE', #5540, #18733, #9530 ) ;
#11872 = CARTESIAN_POINT ( 'NONE',  ( -2.059766911846999893, 13.39089224444999360, -5.755068626256005793 ) ) ;
#11873 = CARTESIAN_POINT ( 'NONE',  ( 0.000000000000000000, 27.25000000000000000, 0.000000000000000000 ) ) ;
#11874 = EDGE_CURVE ( 'NONE', #11018, #19420, #3884, .T. ) ;
#11875 = CARTESIAN_POINT ( 'NONE',  ( 11.97297107871654731, -4.846971342278104444, 12.50004942866789470 ) ) ;
#11876 = CARTESIAN_POINT ( 'NONE',  ( 18.15556881350096319, 8.256286803634841576, -6.419835422307386352 ) ) ;
#11877 = VECTOR ( 'NONE', #8536, 1000.000000000000114 ) ;
#11878 = CARTESIAN_POINT ( 'NONE',  ( -14.25395417760000072, -13.93375672974000068, 0.7213694211268999457 ) ) ;
#11879 = DIRECTION ( 'NONE',  ( -1.000000000000000000, 0.000000000000000000, 0.000000000000000000 ) ) ;
#11880 = DIRECTION ( 'NONE',  ( 0.000000000000000000, -1.000000000000000000, 1.493818482293000218E-14 ) ) ;
#11881 = VERTEX_POINT ( 'NONE', #10126 ) ;
#11882 = CARTESIAN_POINT ( 'NONE',  ( -24.50000000000000355, -4.232391308703559396, -9.760415500123547972 ) ) ;
#11883 = CARTESIAN_POINT ( 'NONE',  ( 4.749999673578000348, 12.55004296393999930, -4.341645649670000483E-06 ) ) ;
#11884 = ORIENTED_EDGE ( 'NONE', *, *, #22074, .T. ) ;
#11885 = CARTESIAN_POINT ( 'NONE',  ( -5.458329129694160287, 16.11242751627741043, -2.784599576127760656 ) ) ;
#11886 = CARTESIAN_POINT ( 'NONE',  ( 2.500000000000000000, 28.63419673618999894, 0.000000000000000000 ) ) ;
#11887 = CARTESIAN_POINT ( 'NONE',  ( 2.707574462781773050, 13.05161192232940870, 6.163505927546630403 ) ) ;
#11888 = AXIS2_PLACEMENT_3D ( 'NONE', #17178, #18647, #13300 ) ;
#11889 = CARTESIAN_POINT ( 'NONE',  ( 1.699999999999999956, 11.63334134365700123, -1.053568440557163255 ) ) ;
#11890 = DIRECTION ( 'NONE',  ( 0.000000000000000000, 1.000000000000000000, 0.000000000000000000 ) ) ;
#11891 = EDGE_CURVE ( 'NONE', #20808, #7660, #2616, .T. ) ;
#11892 = FACE_OUTER_BOUND ( 'NONE', #18044, .T. ) ;
#11893 = EDGE_LOOP ( 'NONE', ( #21580, #13288 ) ) ;
#11894 = CIRCLE ( 'NONE', #3767, 2.100000000000000089 ) ;
#11895 = ORIENTED_EDGE ( 'NONE', *, *, #5231, .F. ) ;
#11896 = CARTESIAN_POINT ( 'NONE',  ( -14.00000000000000355, -7.692389098372126810, -6.335209552320772985 ) ) ;
#11897 = CARTESIAN_POINT ( 'NONE',  ( 2.329590180150573175, 24.49999999999984368, 3.273812635905912316 ) ) ;
#11898 = CARTESIAN_POINT ( 'NONE',  ( -10.04281598263999875, 20.50000000000000000, -1.000000000000000000 ) ) ;
#11899 = CIRCLE ( 'NONE', #23496, 10.59999999999999964 ) ;
#11900 = ORIENTED_EDGE ( 'NONE', *, *, #19338, .F. ) ;
#11901 = CARTESIAN_POINT ( 'NONE',  ( -23.27390197746000311, 9.786885249677000687, 3.008867104030000128 ) ) ;
#11902 = CARTESIAN_POINT ( 'NONE',  ( 0.000000000000000000, 29.69999999999999929, 0.000000000000000000 ) ) ;
#11903 = CARTESIAN_POINT ( 'NONE',  ( -2.000000000000000000, 23.50000000000000000, 0.000000000000000000 ) ) ;
#11904 = CARTESIAN_POINT ( 'NONE',  ( 15.66712465133541698, -8.871746670583112504, 5.331234943396478521 ) ) ;
#11905 = CARTESIAN_POINT ( 'NONE',  ( -17.62205418190999850, -9.739724721154001230, -5.304212073993999077 ) ) ;
#11906 = LINE ( 'NONE', #15636, #6034 ) ;
#11907 = ADVANCED_FACE ( 'NONE', ( #4805 ), #741, .F. ) ;
#11908 = CARTESIAN_POINT ( 'NONE',  ( -19.58358649291538711, -9.522198621325964396, 4.381512970191762335 ) ) ;
#11909 = AXIS2_PLACEMENT_3D ( 'NONE', #18242, #21518, #6976 ) ;
#11910 = B_SPLINE_CURVE_WITH_KNOTS ( 'NONE', 3,
 ( #6212, #2714, #13968, #21359, #4775 ),
 .UNSPECIFIED., .F., .F.,
 ( 4, 1, 4 ),
 ( 0.000000000000000000, 0.5000000000000000000, 1.000000000000000000 ),
 .UNSPECIFIED. ) ;
#11911 = CARTESIAN_POINT ( 'NONE',  ( -17.09903927815000202, -2.106860712391000146, -11.18744719158000045 ) ) ;
#11912 = CARTESIAN_POINT ( 'NONE',  ( -2.024508947676616266, 29.44926370956269324, 0.7533795805217576858 ) ) ;
#11913 = ORIENTED_EDGE ( 'NONE', *, *, #8518, .T. ) ;
#11914 = CARTESIAN_POINT ( 'NONE',  ( -0.7536363891467999787, 23.78037720585000159, 2.224703581606000125 ) ) ;
#11915 = CARTESIAN_POINT ( 'NONE',  ( -15.79421666743139063, -10.31181917561241868, -1.322403086089456226 ) ) ;
#11916 = ORIENTED_EDGE ( 'NONE', *, *, #6245, .T. ) ;
#11917 = CARTESIAN_POINT ( 'NONE',  ( -24.12232999016000079, 1.520060141252000183E-14, 0.000000000000000000 ) ) ;
#11918 = CARTESIAN_POINT ( 'NONE',  ( 5.081337163470998952, 13.95839723273002342, -4.282365589915004378 ) ) ;
#11919 = CARTESIAN_POINT ( 'NONE',  ( 12.00000000000000000, -7.784405687158085563, -4.546983378751352056 ) ) ;
#11920 = DIRECTION ( 'NONE',  ( 0.000000000000000000, 1.000000000000000000, 0.000000000000000000 ) ) ;
#11921 = EDGE_CURVE ( 'NONE', #14445, #709, #18164, .T. ) ;
#11922 = CARTESIAN_POINT ( 'NONE',  ( 15.80625142131000160, 5.282396774718000287, -8.133049213409000444 ) ) ;
#11923 = EDGE_CURVE ( 'NONE', #13362, #4875, #8674, .T. ) ;
#11924 = ORIENTED_EDGE ( 'NONE', *, *, #4638, .F. ) ;
#11925 = CARTESIAN_POINT ( 'NONE',  ( 11.00000000000000000, 0.000000000000000000, 0.000000000000000000 ) ) ;
#11926 = VECTOR ( 'NONE', #22070, 1000.000000000000000 ) ;
#11927 = CARTESIAN_POINT ( 'NONE',  ( 2.434931691670788823, 26.83333333333333570, -0.6543697108982009514 ) ) ;
#11928 = PRODUCT_DEFINITION_SHAPE ( 'NONE', 'NONE',  #2646 ) ;
#11929 = ORIENTED_EDGE ( 'NONE', *, *, #4195, .T. ) ;
#11930 = DIRECTION ( 'NONE',  ( 0.000000000000000000, -0.7071067811866525998, -0.7071067811864425456 ) ) ;
#11931 = CARTESIAN_POINT ( 'NONE',  ( 21.05799999999999983, 9.211671496174000495, 0.000000000000000000 ) ) ;
#11932 = CARTESIAN_POINT ( 'NONE',  ( 0.000000000000000000, 16.89999999999999858, 0.000000000000000000 ) ) ;
#11933 = DIRECTION ( 'NONE',  ( 1.000000000000000000, 0.000000000000000000, 0.000000000000000000 ) ) ;
#11934 = CARTESIAN_POINT ( 'NONE',  ( 18.09556522515502763, 0.2122117348836315975, -10.42041577245926121 ) ) ;
#11935 = VECTOR ( 'NONE', #10300, 1000.000000000000000 ) ;
#11936 = CARTESIAN_POINT ( 'NONE',  ( 12.00000000000000000, -9.392874664203999302, -3.575135015595999999 ) ) ;
#11937 = CONICAL_SURFACE ( 'NONE', #19294, 4.699999872533999756, 0.7853981633972997312 ) ;
#11938 = CARTESIAN_POINT ( 'NONE',  ( -14.49454819745151823, -10.30763366377482804, 7.146668779541629490 ) ) ;
#11940 = EDGE_CURVE ( 'NONE', #12473, #4875, #5345, .T. ) ;
#11939 = CARTESIAN_POINT ( 'NONE',  ( 24.57842594718999862, -9.519849028365999999, 5.132192201719999680 ) ) ;
#11941 = EDGE_CURVE ( 'NONE', #21303, #6884, #22947, .T. ) ;
#11942 = CARTESIAN_POINT ( 'NONE',  ( -2.000000000000000000, 26.50000000000000355, 3.464101615137999968 ) ) ;
#11943 = FACE_OUTER_BOUND ( 'NONE', #15871, .T. ) ;
#11944 = CARTESIAN_POINT ( 'NONE',  ( -2.088094669011058890, 30.23733246308190559, 0.5613753303782254012 ) ) ;
#11945 = ORIENTED_EDGE ( 'NONE', *, *, #20942, .F. ) ;
#11946 = CARTESIAN_POINT ( 'NONE',  ( 21.05259007015999728, -8.871572192553999869, -6.301471715339999946 ) ) ;
#11947 = CARTESIAN_POINT ( 'NONE',  ( 1.757374578699382184, 12.90728621817367028, -6.460611937468210719 ) ) ;
#11948 = CARTESIAN_POINT ( 'NONE',  ( 5.625000000000000000, 22.00000000000000000, 0.000000000000000000 ) ) ;
#11949 = VECTOR ( 'NONE', #21244, 1000.000000000000000 ) ;
#11950 = CARTESIAN_POINT ( 'NONE',  ( -19.65354853982566397, -2.165949038814164673, 10.25715202507329948 ) ) ;
#11951 = DIRECTION ( 'NONE',  ( 0.000000000000000000, 0.7071067811866525998, -0.7071067811864425456 ) ) ;
#11952 = CARTESIAN_POINT ( 'NONE',  ( -2.801175654530000614, 11.78395597969999464, -4.055686653598001179 ) ) ;
#11953 = VERTEX_POINT ( 'NONE', #15919 ) ;
#11954 = CIRCLE ( 'NONE', #13859, 0.09999999999999939493 ) ;
#11955 = CARTESIAN_POINT ( 'NONE',  ( -19.21947896700662639, -10.37017577041856242, -1.473655227643129839 ) ) ;
#11956 = CARTESIAN_POINT ( 'NONE',  ( -4.000000000000000000, 30.00000000000000355, -0.1857058784358550652 ) ) ;
#11957 = CARTESIAN_POINT ( 'NONE',  ( -2.163866556553845744, 27.61887052311726976, -0.1841620332587457221 ) ) ;
#11958 = VERTEX_POINT ( 'NONE', #23432 ) ;
#11959 = VERTEX_POINT ( 'NONE', #17515 ) ;
#11960 = CARTESIAN_POINT ( 'NONE',  ( 17.22299770046334189, -1.193049601325050224, -9.113257778775379236 ) ) ;
#11961 = VECTOR ( 'NONE', #11824, 1000.000000000000000 ) ;
#11962 = CARTESIAN_POINT ( 'NONE',  ( 12.10331408531000008, -5.154040300995999857, -8.697259314724000490 ) ) ;
#11963 = CARTESIAN_POINT ( 'NONE',  ( -23.25600457815999889, -7.940956846984001061, 7.903779492682001084 ) ) ;
#11964 = CARTESIAN_POINT ( 'NONE',  ( -14.47646183292000011, -10.21069195510999883, -0.7742164398386000013 ) ) ;
#11965 = CARTESIAN_POINT ( 'NONE',  ( -1.350644574833474776, 24.52555747447238588, 3.839035148322985425 ) ) ;
#11966 = CARTESIAN_POINT ( 'NONE',  ( 17.02119494526000310, 8.035509840822999905, -6.467739846315000207 ) ) ;
#11967 = CARTESIAN_POINT ( 'NONE',  ( -0.2249661094972814634, 28.79125399117670270, 2.160068143722255307 ) ) ;
#11968 = CARTESIAN_POINT ( 'NONE',  ( -0.6543697108981929578, 26.80086340285666680, 2.434931691670791487 ) ) ;
#11969 = DIRECTION ( 'NONE',  ( 1.000000000000000000, 0.000000000000000000, 0.000000000000000000 ) ) ;
#11970 = AXIS2_PLACEMENT_3D ( 'NONE', #22762, #843, #3046 ) ;
#11971 = CARTESIAN_POINT ( 'NONE',  ( 5.155702020191999857, 13.97328941143999970, -4.008166040501000893 ) ) ;
#11972 = ORIENTED_EDGE ( 'NONE', *, *, #9972, .T. ) ;
#11973 = CARTESIAN_POINT ( 'NONE',  ( 1.455334549417839130, 13.79506959216120343, 5.949608132610088695 ) ) ;
#11974 = CARTESIAN_POINT ( 'NONE',  ( -1.938452583514000072, 27.93413313894999916, 1.528152797339000113 ) ) ;
#11975 = VECTOR ( 'NONE', #23115, 1000.000000000000000 ) ;
#11976 = AXIS2_PLACEMENT_3D ( 'NONE', #19291, #22222, #13020 ) ;
#11977 = CARTESIAN_POINT ( 'NONE',  ( 2.299232923512000593, 11.73080725892999787, 4.209277167837999656 ) ) ;
#11978 = CARTESIAN_POINT ( 'NONE',  ( 0.4257810925096244814, 28.82890265351812431, 2.127227403366187986 ) ) ;
#11979 = CARTESIAN_POINT ( 'NONE',  ( -4.649999999999999467, 20.00000000000000000, 0.000000000000000000 ) ) ;
#11980 = CARTESIAN_POINT ( 'NONE',  ( -6.637070260807000466, 27.93157662065900126, 1.000000000000000000 ) ) ;
#11981 = ORIENTED_EDGE ( 'NONE', *, *, #13868, .F. ) ;
#11982 = CARTESIAN_POINT ( 'NONE',  ( 15.52237270046331830, 2.373835617566403489, -8.833607132019553276 ) ) ;
#11983 = DIRECTION ( 'NONE',  ( -1.000000000000000000, 2.869195662841999727E-10, -3.826635294907999820E-14 ) ) ;
#11984 = CARTESIAN_POINT ( 'NONE',  ( -0.4432754260544001790, 13.79882529351002241, 6.151150798201001635 ) ) ;
#11985 = CARTESIAN_POINT ( 'NONE',  ( 6.356497079780072168E-07, 30.81706029784504963, -2.183072574220335849 ) ) ;
#11986 = DIRECTION ( 'NONE',  ( -0.000000000000000000, 1.000000000000000000, 0.000000000000000000 ) ) ;
#11987 = AXIS2_PLACEMENT_3D ( 'NONE', #23691, #14489, #21881 ) ;
#11988 = CARTESIAN_POINT ( 'NONE',  ( -12.23630863876999975, 8.849960763674998176, -12.38048805091999860 ) ) ;
#11989 = CARTESIAN_POINT ( 'NONE',  ( -15.47399649439000058, -8.448196802485998802, -7.562854223976000156 ) ) ;
#11990 = CARTESIAN_POINT ( 'NONE',  ( 15.56043875731000092, 5.001549981505999831, -7.700678710662999471 ) ) ;
#11991 = CARTESIAN_POINT ( 'NONE',  ( 18.94629248412468314, 1.889948409553210196, 10.26455889571793811 ) ) ;
#11992 = EDGE_LOOP ( 'NONE', ( #22157, #2440, #11473, #5670 ) ) ;
#11993 = CARTESIAN_POINT ( 'NONE',  ( -22.11582036142275243, -8.073955378484633627, 4.653000851119870163 ) ) ;
#11994 = CARTESIAN_POINT ( 'NONE',  ( 2.520990829206000150, 30.76687396097999638, -0.2444226712511999577 ) ) ;
#11995 = CARTESIAN_POINT ( 'NONE',  ( -12.35782654106666634, 6.613167033160651798, -13.46344878000693335 ) ) ;
#11996 = CARTESIAN_POINT ( 'NONE',  ( 1.271172506183420259, 13.76972512329144571, -5.992853696390493923 ) ) ;
#11997 = CIRCLE ( 'NONE', #17815, 4.000000000000000000 ) ;
#11998 = B_SPLINE_CURVE_WITH_KNOTS ( 'NONE', 3,
 ( #21984, #23680, #16524, #14815, #10855 ),
 .UNSPECIFIED., .F., .F.,
 ( 4, 1, 4 ),
 ( 0.000000000000000000, 0.5000000000000000000, 1.000000000000000000 ),
 .UNSPECIFIED. ) ;
#11999 = CARTESIAN_POINT ( 'NONE',  ( 5.267432092546001421, 13.90546002103000056, -3.709299984792997495 ) ) ;
#12000 = CARTESIAN_POINT ( 'NONE',  ( 21.26191220262000314, -10.18341492801999948, 4.724734105908999560 ) ) ;
#12001 = DIRECTION ( 'NONE',  ( 1.000000000000000000, 0.000000000000000000, 0.000000000000000000 ) ) ;
#12002 = CARTESIAN_POINT ( 'NONE',  ( -23.85040575352566350, -5.911899685930855242, 7.659340654891490630 ) ) ;
#12003 = CARTESIAN_POINT ( 'NONE',  ( 15.98114737690458931, -3.455263148493648462, -9.811776265688715526 ) ) ;
#12004 = CARTESIAN_POINT ( 'NONE',  ( 12.52688711657000020, -7.716878364870000340, -11.63397459621999985 ) ) ;
#12005 = DIRECTION ( 'NONE',  ( -1.000000000000000000, 0.000000000000000000, 0.000000000000000000 ) ) ;
#12006 = EDGE_CURVE ( 'NONE', #20571, #14280, #23311, .T. ) ;
#12007 =( BOUNDED_SURFACE ( )  B_SPLINE_SURFACE ( 3, 3, ( 
 ( #6032, #11506, #108, #7860, #13422, #20821, #4232, #18994, #2404, #22742, #6159, #20347, #3754 ),
 ( #15593, #22981, #2778, #15478, #2524, #22862, #4347, #8470, #4595, #9914, #12106, #11738, #6276 ),
 ( #13659, #8342, #6396, #10165, #3022, #10281, #1070, #1197, #21055, #17548, #17671, #17302, #15836 ),
 ( #19613, #4719, #15708, #4468, #13779, #21180, #11984, #6639, #23226, #2653, #945, #23099, #19112 ) ),
 .UNSPECIFIED., .F., .F., .T. ) 
 B_SPLINE_SURFACE_WITH_KNOTS ( ( 4, 4 ),
 ( 4, 1, 1, 1, 1, 1, 1, 1, 1, 1, 4 ),
 ( 0.000000000000000000, 1.000000000000000000 ),
 ( 0.2731447329273000157, 0.2887972725788000017, 0.3269706604050000021, 0.3700588552437000245, 0.4191490422699000185, 0.4751505887952999774, 0.5373493534070999944, 0.6034834658143000130, 0.6714119343383999627, 0.7375481631143000483, 0.7972330670102999450 ),
 .UNSPECIFIED. ) 
 GEOMETRIC_REPRESENTATION_ITEM ( )  RATIONAL_B_SPLINE_SURFACE ( (
 ( 1.179586311108000052, 1.179586311108000052, 1.179586311108000052, 1.179586311108000052, 1.179586311108000052, 1.179586311108000052, 1.179586311108000052, 1.179586311108000052, 1.179586311108000052, 1.179586311108000052, 1.179586311108000052, 1.179586311108000052, 1.179586311108000052),
 ( 0.9401378962973999664, 0.9401378962973999664, 0.9401378962973999664, 0.9401378962973999664, 0.9401378962973999664, 0.9401378962973999664, 0.9401378962973999664, 0.9401378962973999664, 0.9401378962973999664, 0.9401378962973999664, 0.9401378962973999664, 0.9401378962973999664, 0.9401378962973999664),
 ( 0.9401378962973999664, 0.9401378962973999664, 0.9401378962973999664, 0.9401378962973999664, 0.9401378962973999664, 0.9401378962973999664, 0.9401378962973999664, 0.9401378962973999664, 0.9401378962973999664, 0.9401378962973999664, 0.9401378962973999664, 0.9401378962973999664, 0.9401378962973999664),
 ( 1.179586311108000052, 1.179586311108000052, 1.179586311108000052, 1.179586311108000052, 1.179586311108000052, 1.179586311108000052, 1.179586311108000052, 1.179586311108000052, 1.179586311108000052, 1.179586311108000052, 1.179586311108000052, 1.179586311108000052, 1.179586311108000052) ) ) 
 REPRESENTATION_ITEM ( '' )  SURFACE ( )  );
#12008 = CARTESIAN_POINT ( 'NONE',  ( 19.52828936713000019, 9.172416106433001204, 0.000000000000000000 ) ) ;
#12009 = ORIENTED_EDGE ( 'NONE', *, *, #4500, .F. ) ;
#12010 = CARTESIAN_POINT ( 'NONE',  ( -24.50000000000000711, -9.452605432706508992, -4.381486995578353749 ) ) ;
#12011 = CARTESIAN_POINT ( 'NONE',  ( -4.749965457312494088, 12.54998638856619486, -0.6287771473730588978 ) ) ;
#12012 = ORIENTED_EDGE ( 'NONE', *, *, #15854, .T. ) ;
#12013 = CARTESIAN_POINT ( 'NONE',  ( 1.709999999999999964, 9.000000000000000000, 7.500000000000000000 ) ) ;
#12014 = CARTESIAN_POINT ( 'NONE',  ( 23.41677564524290744, 34.01856778792605240, 6.000000000000000000 ) ) ;
#12015 = CARTESIAN_POINT ( 'NONE',  ( -1.216511548453131253, 12.85264031799866835, 6.568461162512661211 ) ) ;
#12016 = B_SPLINE_CURVE_WITH_KNOTS ( 'NONE', 3,
 ( #21916, #7368, #9077, #14867, #12600, #22149, #5671, #1927, #12830, #5560, #20111, #1462, #13059, #16337 ),
 .UNSPECIFIED., .F., .F.,
 ( 4, 1, 1, 1, 1, 1, 1, 2, 2, 4 ),
 ( 0.000000000000000000, 0.2499999999999956701, 0.3749999999999936162, 0.4374999999999925060, 0.4687499999999916178, 0.4843749999999909517, 0.4921874999999909517, 0.4960937499999911737, 0.4999999999999914513, 1.000000000000000000 ),
 .UNSPECIFIED. ) ;
#12017 = CARTESIAN_POINT ( 'NONE',  ( 15.67432937369000001, -6.527804446355999879, 8.913017593376000747 ) ) ;
#12018 = DIRECTION ( 'NONE',  ( 0.000000000000000000, -1.000000000000000000, 0.000000000000000000 ) ) ;
#12019 = CARTESIAN_POINT ( 'NONE',  ( 24.50000000000000000, 4.174438572590999431E-14, -12.50000000000000000 ) ) ;
#12020 = ADVANCED_FACE ( 'NONE', ( #17397 ), #21638, .T. ) ;
#12021 = ORIENTED_EDGE ( 'NONE', *, *, #12899, .F. ) ;
#12022 = ORIENTED_EDGE ( 'NONE', *, *, #21424, .T. ) ;
#12023 = FACE_OUTER_BOUND ( 'NONE', #8352, .T. ) ;
#12024 = CARTESIAN_POINT ( 'NONE',  ( 2.000000000000000000, 24.50000000000000000, 3.464101615137999968 ) ) ;
#12025 = CARTESIAN_POINT ( 'NONE',  ( -6.706871426378296697, 15.26719126503497215, -2.301088630243747879 ) ) ;
#12026 = ORIENTED_EDGE ( 'NONE', *, *, #17664, .F. ) ;
#12027 = PLANE ( 'NONE',  #9016 ) ;
#12028 = CARTESIAN_POINT ( 'NONE',  ( 24.00034722001000276, 6.716786536054000223, -12.21137788280000080 ) ) ;
#12029 = CARTESIAN_POINT ( 'NONE',  ( 14.97832412782650380, 10.09172200828920474, 2.218384077932363141 ) ) ;
#12030 = CARTESIAN_POINT ( 'NONE',  ( -16.21078937980000134, -1.833411044341999974, 10.89860299424000090 ) ) ;
#12031 = CARTESIAN_POINT ( 'NONE',  ( -1.057980244643000001, 29.08125461216999952, -2.105335631596999768 ) ) ;
#12032 = CARTESIAN_POINT ( 'NONE',  ( -20.30417001384837761, 10.26022708029042008, 2.230831165255982018 ) ) ;
#12033 = CARTESIAN_POINT ( 'NONE',  ( 4.725446626782000337, 12.53698071169998762, -0.1085052580315999798 ) ) ;
#12034 = CARTESIAN_POINT ( 'NONE',  ( 2.500000000000000000, 29.43419673618999965, 0.000000000000000000 ) ) ;
#12035 = EDGE_CURVE ( 'NONE', #16279, #13125, #20861, .T. ) ;
#12036 = CARTESIAN_POINT ( 'NONE',  ( -1.851996671504216430, 29.47254427382508268, 1.111577618485255048 ) ) ;
#12037 = ORIENTED_EDGE ( 'NONE', *, *, #362, .T. ) ;
#12038 = CARTESIAN_POINT ( 'NONE',  ( 0.9155365142161999703, 24.93361692991000211, -1.984919506156000324 ) ) ;
#12039 = CARTESIAN_POINT ( 'NONE',  ( -15.01285897352482301, 9.893965164599533679, -3.127973572333462293 ) ) ;
#12040 = VECTOR ( 'NONE', #5321, 1000.000000000000000 ) ;
#12041 = ORIENTED_EDGE ( 'NONE', *, *, #23568, .T. ) ;
#12042 = CARTESIAN_POINT ( 'NONE',  ( 5.921804960513004090, 14.11680711012999367, -1.397333608379999204 ) ) ;
#12043 = CARTESIAN_POINT ( 'NONE',  ( 12.00000000000000355, -1.539276415234435369, -8.846422256191463163 ) ) ;
#12044 = CARTESIAN_POINT ( 'NONE',  ( -19.69192920454666051, 8.018450232194952676, -4.621400420351030824 ) ) ;
#12045 = ADVANCED_FACE ( 'NONE', ( #7319 ), #5278, .T. ) ;
#12046 = CARTESIAN_POINT ( 'NONE',  ( 13.28343892131000104, -9.177482186369001482, 2.922696180057999804 ) ) ;
#12047 = ORIENTED_EDGE ( 'NONE', *, *, #2289, .T. ) ;
#12048 = CARTESIAN_POINT ( 'NONE',  ( 5.699442596042000098, 1.578914512950999657E-14, 0.000000000000000000 ) ) ;
#12049 = CARTESIAN_POINT ( 'NONE',  ( -2.500000000000000000, 27.19999999999999929, 0.000000000000000000 ) ) ;
#12050 = DIRECTION ( 'NONE',  ( 0.000000000000000000, 1.000000000000000000, 0.000000000000000000 ) ) ;
#12051 = ORIENTED_EDGE ( 'NONE', *, *, #11921, .F. ) ;
#12052 = CYLINDRICAL_SURFACE ( 'NONE', #5741, 1.000000000000000000 ) ;
#12053 = CARTESIAN_POINT ( 'NONE',  ( 11.48696334737391034, 9.189637287616163164, 9.082924181322448831 ) ) ;
#12054 = CARTESIAN_POINT ( 'NONE',  ( -23.30805980735596350, 8.264335043300832240, -4.289310384929161835 ) ) ;
#12055 = CARTESIAN_POINT ( 'NONE',  ( 24.50000000000000000, 0.000000000000000000, 0.000000000000000000 ) ) ;
#12056 = CARTESIAN_POINT ( 'NONE',  ( 16.45228901489213058, 5.938338979451788013, -8.534682244571794030 ) ) ;
#12057 = EDGE_CURVE ( 'NONE', #8075, #18038, #10433, .T. ) ;
#12058 = DIRECTION ( 'NONE',  ( -1.000000000000000000, 0.000000000000000000, 0.000000000000000000 ) ) ;
#12059 = CARTESIAN_POINT ( 'NONE',  ( -14.48092000065305385, 9.982182315252655869, -7.710362946291708930 ) ) ;
#12060 = CARTESIAN_POINT ( 'NONE',  ( 20.63850044899999858, -5.380123924041000372, 9.833381923714000550 ) ) ;
#12061 = CARTESIAN_POINT ( 'NONE',  ( 4.000000000000000000, 28.30000000000000071, 2.309401076759000304 ) ) ;
#12062 = CARTESIAN_POINT ( 'NONE',  ( -4.111914283818391525, 13.74838725675451379, -4.878539065083999482 ) ) ;
#12063 = CARTESIAN_POINT ( 'NONE',  ( 12.49102043323999922, 6.966843713870000343, -12.06700730386999965 ) ) ;
#12064 = ADVANCED_FACE ( 'NONE', ( #16642 ), #23946, .F. ) ;
#12065 = CARTESIAN_POINT ( 'NONE',  ( -1.284157455750906118, 30.08499832656240258, -1.737012890293607503 ) ) ;
#12066 = EDGE_LOOP ( 'NONE', ( #1262, #6009, #23341, #18076 ) ) ;
#12067 = EDGE_CURVE ( 'NONE', #4069, #2201, #14558, .T. ) ;
#12068 = CARTESIAN_POINT ( 'NONE',  ( 23.17332811867109754, 4.643914442280755672, 8.043476694703691976 ) ) ;
#12069 = CARTESIAN_POINT ( 'NONE',  ( 23.75810313999999934, 9.259900066636999938, 5.856734761124000599 ) ) ;
#12070 = CARTESIAN_POINT ( 'NONE',  ( 12.52688711657000020, 6.216878364870000340, -12.50000000000000000 ) ) ;
#12071 = DIRECTION ( 'NONE',  ( -1.000000000000000000, 0.000000000000000000, 0.000000000000000000 ) ) ;
#12072 = CARTESIAN_POINT ( 'NONE',  ( -0.8506511933622447064, 24.58106360703828841, 2.086532260108333592 ) ) ;
#12073 = CARTESIAN_POINT ( 'NONE',  ( 4.846185023065524788, 14.59761631344303545, 3.777028798763933715 ) ) ;
#12074 = CARTESIAN_POINT ( 'NONE',  ( -3.690048612459000843, 12.01986709263998598, -3.260388994065002155 ) ) ;
#12075 = VERTEX_POINT ( 'NONE', #11080 ) ;
#12076 = CARTESIAN_POINT ( 'NONE',  ( -15.89804173673989318, -6.399027050157823027, 8.374265193961687004 ) ) ;
#12077 = VECTOR ( 'NONE', #732, 1000.000000000000000 ) ;
#12078 = ADVANCED_FACE ( 'NONE', ( #18348 ), #23791, .F. ) ;
#12079 = CARTESIAN_POINT ( 'NONE',  ( 23.99062354302999722, 13.93375672974000068, 0.8660254037843999608 ) ) ;
#12080 = CARTESIAN_POINT ( 'NONE',  ( 0.7890445379464539055, 26.58333480217339684, -2.052919754909737104 ) ) ;
#12081 = DIRECTION ( 'NONE',  ( 1.000000000000000000, 0.000000000000000000, 0.000000000000000000 ) ) ;
#12082 = DIRECTION ( 'NONE',  ( 0.000000000000000000, 1.000000000000000000, 0.000000000000000000 ) ) ;
#12083 = ORIENTED_EDGE ( 'NONE', *, *, #19584, .T. ) ;
#12084 = CARTESIAN_POINT ( 'NONE',  ( 17.52533103379666812, 7.293684496933804162, -5.605380383579831260 ) ) ;
#12085 = AXIS2_PLACEMENT_3D ( 'NONE', #15958, #3030, #10417 ) ;
#12086 = CARTESIAN_POINT ( 'NONE',  ( -5.101723131807428757, 15.93850954079848670, -3.397737009563421839 ) ) ;
#12087 = CARTESIAN_POINT ( 'NONE',  ( -24.00694541842999996, 8.257142182343001124, 6.813018789841999379 ) ) ;
#12088 = CARTESIAN_POINT ( 'NONE',  ( -15.83232383131000276, -8.056602140089001551, -7.212379830447999574 ) ) ;
#12089 = CARTESIAN_POINT ( 'NONE',  ( -6.124356664509996051, 15.85446180679002559, 1.061635727481998748 ) ) ;
#12090 = CARTESIAN_POINT ( 'NONE',  ( 16.00556994525999954, -5.082985426985000110, 8.943222925845001114 ) ) ;
#12091 = CARTESIAN_POINT ( 'NONE',  ( -14.25395396059999875, -13.93375672974000068, -0.7213900596348999938 ) ) ;
#12092 = CARTESIAN_POINT ( 'NONE',  ( -14.25699038479000080, 13.93375672974000068, 0.1445756673977000029 ) ) ;
#12093 = EDGE_CURVE ( 'NONE', #22144, #11065, #11998, .T. ) ;
#12094 = DIRECTION ( 'NONE',  ( 0.000000000000000000, 1.000000000000000000, 0.000000000000000000 ) ) ;
#12095 = VERTEX_POINT ( 'NONE', #21869 ) ;
#12096 = CARTESIAN_POINT ( 'NONE',  ( -3.371625728408081279, 14.23819322435518053, 5.124742718149488674 ) ) ;
#12097 = CARTESIAN_POINT ( 'NONE',  ( 2.467893978438000069, 27.44663313894999845, 0.04846321314148000631 ) ) ;
#12098 = CIRCLE ( 'NONE', #10561, 7.100000000000000533 ) ;
#12099 = CARTESIAN_POINT ( 'NONE',  ( -19.96237077250665237, -7.343695055788383108, -5.643813670142061589 ) ) ;
#12100 = CARTESIAN_POINT ( 'NONE',  ( -2.370125023230000405, 28.58187716036000126, -0.6185023500890999282 ) ) ;
#12101 = DIRECTION ( 'NONE',  ( 1.000000000000000000, 0.000000000000000000, 0.000000000000000000 ) ) ;
#12102 = VERTEX_POINT ( 'NONE', #18237 ) ;
#12103 = CARTESIAN_POINT ( 'NONE',  ( -3.000000000000000000, 15.00000000000000000, 0.000000000000000000 ) ) ;
#12104 = DIRECTION ( 'NONE',  ( 0.000000000000000000, 0.000000000000000000, -1.000000000000000000 ) ) ;
#12105 = ADVANCED_FACE ( 'NONE', ( #18466 ), #21119, .F. ) ;
#12106 = CARTESIAN_POINT ( 'NONE',  ( 4.505994758382000143, 13.58051267175999044, 4.661972778555996122 ) ) ;
#12107 = CARTESIAN_POINT ( 'NONE',  ( -0.2074533927172730330, 30.82465819688974662, -2.175341810225499550 ) ) ;
#12108 = LINE ( 'NONE', #8344, #20411 ) ;
#12109 = CARTESIAN_POINT ( 'NONE',  ( -10.59977471169000118, 14.06013194402999922, 6.685927415084999659 ) ) ;
#12110 = CARTESIAN_POINT ( 'NONE',  ( -14.86460545047999915, 10.81390249068999942, -3.353128725732000159 ) ) ;
#12111 = VECTOR ( 'NONE', #18886, 1000.000000000000000 ) ;
#12112 = CARTESIAN_POINT ( 'NONE',  ( 16.98637625730999900, -6.405805545913000110, -6.631092424295999876 ) ) ;
#12113 = CARTESIAN_POINT ( 'NONE',  ( 18.93537196294775882, 2.265043017815088433, 10.18579095625258546 ) ) ;
#12114 = ORIENTED_EDGE ( 'NONE', *, *, #11710, .F. ) ;
#12115 = CARTESIAN_POINT ( 'NONE',  ( -22.66395956040253523, 6.970187874413995566, 6.113416044038686437 ) ) ;
#12116 = CARTESIAN_POINT ( 'NONE',  ( -0.1992920871147000061, 30.85997849182999886, -2.333249878129000088 ) ) ;
#12117 = DIRECTION ( 'NONE',  ( 0.000000000000000000, 0.000000000000000000, 1.000000000000000000 ) ) ;
#12118 = CARTESIAN_POINT ( 'NONE',  ( 2.248479345707985910, 13.93831621736242532, -5.697544554129113870 ) ) ;
#12119 = EDGE_LOOP ( 'NONE', ( #12596, #12780, #21042, #1962 ) ) ;
#12120 = CARTESIAN_POINT ( 'NONE',  ( -1.989999999999999991, 13.00000000000000000, -7.500000000000000000 ) ) ;
#12121 = DIRECTION ( 'NONE',  ( 0.000000000000000000, 1.000000000000000000, 0.000000000000000000 ) ) ;
#12122 = CARTESIAN_POINT ( 'NONE',  ( 1.702290430855999848, 28.68904868065000002, -2.154272664354000000 ) ) ;
#12123 = CARTESIAN_POINT ( 'NONE',  ( 0.000000000000000000, 30.00000000000000000, 0.000000000000000000 ) ) ;
#12124 = CARTESIAN_POINT ( 'NONE',  ( 16.53869133500922572, 10.41447537069648099, 0.2212634277976356645 ) ) ;
#12125 = DIRECTION ( 'NONE',  ( 0.000000000000000000, -1.000000000000000000, 0.000000000000000000 ) ) ;
#12126 = CARTESIAN_POINT ( 'NONE',  ( 0.000000000000000000, 30.00000000000000000, 0.000000000000000000 ) ) ;
#12127 = CARTESIAN_POINT ( 'NONE',  ( 19.56608103379665664, 9.173385915083406061, 1.200666460651664158 ) ) ;
#12128 = VERTEX_POINT ( 'NONE', #2461 ) ;
#12129 = LINE ( 'NONE', #9493, #15444 ) ;
#12130 = CARTESIAN_POINT ( 'NONE',  ( 12.06371966929668282, -8.266677037995437516, 10.68189384375242668 ) ) ;
#12131 = EDGE_LOOP ( 'NONE', ( #13131, #20384, #884 ) ) ;
#12132 = CARTESIAN_POINT ( 'NONE',  ( -1.875449657889999955, 25.64909039007000047, 1.720651897418999932 ) ) ;
#12133 = DIRECTION ( 'NONE',  ( 1.000000000000000000, 0.000000000000000000, 0.000000000000000000 ) ) ;
#12134 = CARTESIAN_POINT ( 'NONE',  ( 2.972536222373345360, 13.09994088774743481, 6.061060134369011365 ) ) ;
#12135 = CARTESIAN_POINT ( 'NONE',  ( 14.59162398661999838, 0.2593516755336999768, -11.01510379984999943 ) ) ;
#12136 = CARTESIAN_POINT ( 'NONE',  ( -20.48587921418834057, -3.712447563501607206, 8.482500515389572726 ) ) ;
#12137 = AXIS2_PLACEMENT_3D ( 'NONE', #4144, #2329, #11306 ) ;
#12138 = DIRECTION ( 'NONE',  ( -0.8181527231370768760, -7.041731039369663653E-17, 0.5750009753238559673 ) ) ;
#12139 = ORIENTED_EDGE ( 'NONE', *, *, #17646, .F. ) ;
#12140 = CARTESIAN_POINT ( 'NONE',  ( -14.00000000000000355, -9.891701185583293920, -2.661512775288601418 ) ) ;
#12141 = CARTESIAN_POINT ( 'NONE',  ( -10.34021276376999943, 1.351277883783999990E-14, 0.000000000000000000 ) ) ;
#12142 = CARTESIAN_POINT ( 'NONE',  ( 12.52688711657000020, -7.716878364870000340, 11.63397459621999985 ) ) ;
#12143 = EDGE_CURVE ( 'NONE', #14442, #13340, #20754, .T. ) ;
#12144 = ORIENTED_EDGE ( 'NONE', *, *, #346, .F. ) ;
#12145 = CARTESIAN_POINT ( 'NONE',  ( -20.43318916570999733, -0.1401826590115999860, -10.68367857704999935 ) ) ;
#12146 = CARTESIAN_POINT ( 'NONE',  ( -24.50000000000000000, -10.82531754731000007, 6.250000000000000000 ) ) ;
#12147 = CARTESIAN_POINT ( 'NONE',  ( 21.05799999999999983, 9.211671496174000495, 0.000000000000000000 ) ) ;
#12148 = CARTESIAN_POINT ( 'NONE',  ( 15.23661952948198817, 4.575606413770517022, 9.271423793378714251 ) ) ;
#12149 = CARTESIAN_POINT ( 'NONE',  ( -16.93344263992999998, 7.982151262181000462, -7.672296569841999592 ) ) ;
#12150 = CARTESIAN_POINT ( 'NONE',  ( -1.958081313796000034, 29.29706567419000152, 1.310602052684999963 ) ) ;
#12151 = FACE_OUTER_BOUND ( 'NONE', #5680, .T. ) ;
#12152 = CARTESIAN_POINT ( 'NONE',  ( -4.735820586438997282, 12.61288540589000640, -0.3245998379664998823 ) ) ;
#12153 = EDGE_LOOP ( 'NONE', ( #13294, #6333, #21845, #9297, #5452 ) ) ;
#12154 = CARTESIAN_POINT ( 'NONE',  ( -24.50000000000000000, -9.995791495354000133, -2.484784171996999635 ) ) ;
#12155 = CARTESIAN_POINT ( 'NONE',  ( -1.832658730057130203, 29.47472325661898651, 1.143358172601616207 ) ) ;
#12156 = ORIENTED_EDGE ( 'NONE', *, *, #18300, .T. ) ;
#12157 = CARTESIAN_POINT ( 'NONE',  ( 0.000000000000000000, 22.10000000618969906, 0.000000000000000000 ) ) ;
#12158 = CARTESIAN_POINT ( 'NONE',  ( -17.32799288139599980, -4.762660099403713154, -9.278735530162990131 ) ) ;
#12159 = VERTEX_POINT ( 'NONE', #19051 ) ;
#12160 = DIRECTION ( 'NONE',  ( 0.000000000000000000, 1.000000000000000000, 0.000000000000000000 ) ) ;
#12161 = CARTESIAN_POINT ( 'NONE',  ( 6.104584092870004142, 13.74269313579999974, -1.459638886711001282 ) ) ;
#12162 = CARTESIAN_POINT ( 'NONE',  ( 12.00000000000000355, -3.246823130105976674, -8.379510835762300047 ) ) ;
#12163 = CARTESIAN_POINT ( 'NONE',  ( -19.84309587121332896, 4.623588645206304193, -8.021742693057086981 ) ) ;
#12164 = CIRCLE ( 'NONE', #20656, 3.000000000000000000 ) ;
#12165 = CARTESIAN_POINT ( 'NONE',  ( 13.20018908531000079, -1.240977706124000157, 10.06232283554999896 ) ) ;
#12166 = ORIENTED_EDGE ( 'NONE', *, *, #3618, .F. ) ;
#12167 = CARTESIAN_POINT ( 'NONE',  ( -9.603671492921000308, -7.945443728446001330, 12.15033259826000034 ) ) ;
#12168 = CARTESIAN_POINT ( 'NONE',  ( 0.000000000000000000, 16.89999999999999858, 0.000000000000000000 ) ) ;
#12169 = CARTESIAN_POINT ( 'NONE',  ( -10.90000000000000036, 1.358133300253999998E-14, 0.000000000000000000 ) ) ;
#12170 = EDGE_CURVE ( 'NONE', #4287, #6758, #19505, .T. ) ;
#12171 = ORIENTED_EDGE ( 'NONE', *, *, #22099, .F. ) ;
#12172 = CARTESIAN_POINT ( 'NONE',  ( 11.18574820343528131, 11.70054794219022476, 4.734095432790576652 ) ) ;
#12173 = CARTESIAN_POINT ( 'NONE',  ( -23.36335304951608904, 7.300808882634314934, -5.780451761111838671 ) ) ;
#12174 = CARTESIAN_POINT ( 'NONE',  ( 1.709999999999999964, 13.00000000000000000, 7.500000000000000000 ) ) ;
#12175 = CARTESIAN_POINT ( 'NONE',  ( 16.24398043996313845, -1.141157097763910278, -10.31439134400806346 ) ) ;
#12176 = CARTESIAN_POINT ( 'NONE',  ( 11.99999999999999822, -8.124792819186978932, -5.670701520036931065 ) ) ;
#12177 = CARTESIAN_POINT ( 'NONE',  ( -14.49454883410026085, -11.27877807214812833, 5.464517788383423280 ) ) ;
#12178 = VECTOR ( 'NONE', #8631, 1000.000000000000000 ) ;
#12179 = CARTESIAN_POINT ( 'NONE',  ( -3.937744478194991515, 13.91798078350775292, -4.847309677219109325 ) ) ;
#12180 = CARTESIAN_POINT ( 'NONE',  ( -24.50000000000293099, 10.69708164072063461, -6.472111105570566458 ) ) ;
#12181 = ADVANCED_FACE ( 'NONE', ( #13132 ), #20527, .T. ) ;
#12182 = CARTESIAN_POINT ( 'NONE',  ( -1.908738021986881250, 30.14178492054505298, -1.010896472074411578 ) ) ;
#12183 = VERTEX_POINT ( 'NONE', #22565 ) ;
#12184 = FACE_OUTER_BOUND ( 'NONE', #9655, .T. ) ;
#12185 = CARTESIAN_POINT ( 'NONE',  ( 24.19716673756000347, 3.808960480925000169, 10.85543100556000162 ) ) ;
#12186 = CARTESIAN_POINT ( 'NONE',  ( 4.000000000000116351, 27.99999999999975842, -0.3805779584833441365 ) ) ;
#12187 = DIRECTION ( 'NONE',  ( 1.000000000000000000, 0.000000000000000000, 0.000000000000000000 ) ) ;
#12188 = AXIS2_PLACEMENT_3D ( 'NONE', #21834, #9000, #21723 ) ;
#12189 = VERTEX_POINT ( 'NONE', #18699 ) ;
#12190 = CARTESIAN_POINT ( 'NONE',  ( -20.67105079060898376, -1.821131150673523491, -10.35028598315374815 ) ) ;
#12191 = DIRECTION ( 'NONE',  ( -1.000000000000000000, 0.000000000000000000, 0.000000000000000000 ) ) ;
#12192 = CARTESIAN_POINT ( 'NONE',  ( -1.474518126777998983, 11.62008507038000715, -4.742463282491001131 ) ) ;
#12193 = ORIENTED_EDGE ( 'NONE', *, *, #19338, .T. ) ;
#12194 = EDGE_CURVE ( 'NONE', #19391, #20571, #3847, .T. ) ;
#12195 = CARTESIAN_POINT ( 'NONE',  ( -16.06550916011372721, -0.7239279268763375574, 10.37154066821624099 ) ) ;
#12196 = CARTESIAN_POINT ( 'NONE',  ( -3.999996093277206732, 24.62756664670158102, -1.519951541552794883 ) ) ;
#12197 = CIRCLE ( 'NONE', #7543, 0.09999999999999982514 ) ;
#12198 = CARTESIAN_POINT ( 'NONE',  ( 2.167090447363087868, 26.42307332155113642, 0.1133437460621688486 ) ) ;
#12199 = PLANE ( 'NONE',  #2078 ) ;
#12200 = ADVANCED_FACE ( 'NONE', ( #278 ), #10163, .F. ) ;
#12201 = ORIENTED_EDGE ( 'NONE', *, *, #3460, .F. ) ;
#12202 = CARTESIAN_POINT ( 'NONE',  ( -23.74465998031000069, 6.216878364870000340, -12.50000000000000000 ) ) ;
#12203 = CARTESIAN_POINT ( 'NONE',  ( -4.421389682918046127, 15.40904240291348692, -4.239377148695758990 ) ) ;
#12204 = CARTESIAN_POINT ( 'NONE',  ( -24.80987884326999904, -5.066946248634999428, -8.838305289106999751 ) ) ;
#12205 = CARTESIAN_POINT ( 'NONE',  ( -18.33593844434000175, -7.737619111796999682, 6.870299314828000270 ) ) ;
#12206 = CARTESIAN_POINT ( 'NONE',  ( 0.000000000000000000, 13.10000000000000142, 0.000000000000000000 ) ) ;
#12207 = CARTESIAN_POINT ( 'NONE',  ( 13.43312451745999958, 0.8166441206667999220, -8.872015940503999332 ) ) ;
#12208 = FACE_BOUND ( 'NONE', #8281, .T. ) ;
#12209 = CARTESIAN_POINT ( 'NONE',  ( 23.99062354302999722, -13.93375672974000068, 0.8660254037843999608 ) ) ;
#12210 = EDGE_CURVE ( 'NONE', #21237, #5409, #17384, .T. ) ;
#12211 = CARTESIAN_POINT ( 'NONE',  ( 15.31366666666666276, 4.564816387457174329, -7.920276097247842095 ) ) ;
#12212 = ORIENTED_EDGE ( 'NONE', *, *, #22531, .F. ) ;
#12213 = CARTESIAN_POINT ( 'NONE',  ( -3.102235637044312266, 14.15615357930589191, 5.289215628019240611 ) ) ;
#12214 = CARTESIAN_POINT ( 'NONE',  ( -1.538852087555999892, 27.04869850837999934, 1.664720809480999986 ) ) ;
#12215 = CIRCLE ( 'NONE', #8333, 1.000000000000000888 ) ;
#12216 = CARTESIAN_POINT ( 'NONE',  ( -19.77341243917331681, -2.402389709466869139, -8.939857867861107366 ) ) ;
#12217 = CARTESIAN_POINT ( 'NONE',  ( -14.50464602252369772, 1.560506203883582632, -8.906515074185010761 ) ) ;
#12218 = CARTESIAN_POINT ( 'NONE',  ( 2.036706090186000129, 28.28937716036000083, -1.360883606431000148 ) ) ;
#12219 = CARTESIAN_POINT ( 'NONE',  ( -3.794133490988780721, 12.08388102651774965, 2.997060710912608172 ) ) ;
#12220 = VERTEX_POINT ( 'NONE', #7550 ) ;
#12221 =( REPRESENTATION_RELATIONSHIP ('NONE','NONE', #13682, #14475 ) REPRESENTATION_RELATIONSHIP_WITH_TRANSFORMATION ( #16293 )SHAPE_REPRESENTATION_RELATIONSHIP( ) );
#12222 = CARTESIAN_POINT ( 'NONE',  ( -7.500000000000000000, 28.00000000000000000, -6.000000000000000000 ) ) ;
#12223 = CARTESIAN_POINT ( 'NONE',  ( 2.616450853603692117, 11.77236066036824091, -4.051655692838156853 ) ) ;
#12224 = LINE ( 'NONE', #21306, #16901 ) ;
#12225 = CARTESIAN_POINT ( 'NONE',  ( 11.51452871203068717, -7.818510255363073647, -4.442849280847243065 ) ) ;
#12226 = PLANE ( 'NONE',  #14228 ) ;
#12227 = EDGE_CURVE ( 'NONE', #19197, #11438, #6084, .T. ) ;
#12228 = AXIS2_PLACEMENT_3D ( 'NONE', #19286, #8022, #15394 ) ;
#12229 = EDGE_CURVE ( 'NONE', #12844, #20964, #9852, .T. ) ;
#12230 = CARTESIAN_POINT ( 'NONE',  ( -1.425617094341268931, 30.52806882488800966, -2.032309464588828885 ) ) ;
#12231 = CARTESIAN_POINT ( 'NONE',  ( -15.67712684235999987, -11.34047394370000106, -0.3014134449561000073 ) ) ;
#12232 = CIRCLE ( 'NONE', #6422, 2.999999999999999112 ) ;
#12233 = CARTESIAN_POINT ( 'NONE',  ( 14.92875142131000210, -6.069959421551999412, 7.533852356441999909 ) ) ;
#12234 = CARTESIAN_POINT ( 'NONE',  ( -0.3272492347489287523, 27.38333333333333997, 2.500000000000001332 ) ) ;
#12235 = B_SPLINE_CURVE_WITH_KNOTS ( 'NONE', 3,
 ( #10244, #21632, #12546, #19575, #10613, #8795, #8307, #15672, #1032, #13871, #16035, #1163, #21274, #15800, #23559, #8557, #17997, #19697, #19453, #23061, #1402, #19932, #23192, #4801, #2980, #16157, #6609, #906, #5051, #3350, #17512, #12307, #12433, #21386, #6489, #10370, #23306, #6723, #14114, #6967, #21509, #3113, #10497, #17882, #1283, #14811, #1636, #12662, #18121, #22205, #16282, #5739, #1754, #8916, #12882, #9261, #13001, #20402, #18585, #9141, #9025, #13128, #7549, #22094, #16519, #3466, #5504, #3575, #7314, #158, #7428, #5619, #22323, #10851, #23906, #3808, #23675, #1989, #14927, #3687, #14703, #7195, #18233, #11204, #14585, #16395, #7083, #9374, #20524, #23787, #20283, #21979, #5393, #12778, #11077, #18461, #20169, #10729, #16746, #1527, #1874, #10958, #18344, #16637, #46, #14470, #21865, #5274, #20050, #2220, #18812, #2805, #2103, #16997, #4491, #19392 ),
 .UNSPECIFIED., .F., .F.,
 ( 4, 2, 2, 2, 2, 2, 1, 2, 2, 2, 2, 2, 2, 2, 2, 2, 2, 2, 2, 2, 2, 2, 2, 2, 2, 2, 2, 2, 2, 2, 2, 2, 2, 2, 2, 2, 2, 2, 2, 2, 2, 2, 2, 2, 2, 2, 2, 2, 2, 2, 2, 2, 1, 2, 2, 2, 2, 2, 4 ),
 ( 0.000000000000000000, 0.01562499999999999653, 0.03124999999999999306, 0.04687499999999998612, 0.06249999999999998612, 0.07812499999999997224, 0.09374999999999997224, 0.1093749999999999584, 0.1249999999999999584, 0.1406249999999999722, 0.1562499999999999722, 0.1718749999999999722, 0.1874999999999999445, 0.2031249999999999445, 0.2187499999999999445, 0.2343749999999999445, 0.2499999999999999445, 0.2656249999999999445, 0.2812499999999999445, 0.2968749999999999445, 0.3124999999999999445, 0.3281249999999999445, 0.3437499999999999445, 0.3593749999999999445, 0.3749999999999998890, 0.3906249999999998890, 0.4062499999999999445, 0.4375000000000000000, 0.4687500000000000555, 0.5000000000000001110, 0.5312500000000001110, 0.5625000000000001110, 0.5937500000000001110, 0.6093750000000001110, 0.6250000000000001110, 0.6406250000000001110, 0.6562500000000001110, 0.6718750000000001110, 0.6875000000000001110, 0.7031250000000001110, 0.7187500000000001110, 0.7343750000000001110, 0.7500000000000000000, 0.7656250000000000000, 0.7812500000000000000, 0.7968750000000000000, 0.8125000000000000000, 0.8281250000000000000, 0.8437500000000000000, 0.8593750000000000000, 0.8750000000000000000, 0.8906250000000000000, 0.9062500000000000000, 0.9218750000000000000, 0.9375000000000000000, 0.9531250000000000000, 0.9687500000000000000, 0.9843750000000000000, 1.000000000000000000 ),
 .UNSPECIFIED. ) ;
#12236 = VERTEX_POINT ( 'NONE', #17231 ) ;
#12237 = CARTESIAN_POINT ( 'NONE',  ( -22.45604469182422136, 1.209830229891543540, 9.246699917977114325 ) ) ;
#12238 = CARTESIAN_POINT ( 'NONE',  ( -2.108931671552999987, 29.74725334348999795, 1.723862884677999974 ) ) ;
#12239 = CARTESIAN_POINT ( 'NONE',  ( -15.46516243917332822, 7.923575937676545777, 4.567008865628563896 ) ) ;
#12240 = CARTESIAN_POINT ( 'NONE',  ( -23.68078907432000335, -9.459496811531000304, -9.754788243598999975E-09 ) ) ;
#12241 = EDGE_LOOP ( 'NONE', ( #8773, #6955, #19919, #8148, #13990 ) ) ;
#12242 = CARTESIAN_POINT ( 'NONE',  ( 2.100000000000000089, 18.89999999999999858, 1.955007544740999697E-10 ) ) ;
#12243 = CARTESIAN_POINT ( 'NONE',  ( 5.302302355349000074, 1.402151973163523525E-14, 14.43375672973994917 ) ) ;
#12244 = LINE ( 'NONE', #1459, #11151 ) ;
#12245 = EDGE_CURVE ( 'NONE', #20167, #1386, #23578, .T. ) ;
#12246 = CARTESIAN_POINT ( 'NONE',  ( 0.6590036730604669213, 24.50443762530719027, -2.307010909781515906 ) ) ;
#12247 = CARTESIAN_POINT ( 'NONE',  ( 16.28779655386367509, 6.890083051547521542, -7.810293348495036092 ) ) ;
#12248 = CARTESIAN_POINT ( 'NONE',  ( -3.688226731973703654, 14.24897469870492372, 4.890359035125574572 ) ) ;
#12249 = CARTESIAN_POINT ( 'NONE',  ( -21.96532910583999865, -9.234955349282000014, 0.000000000000000000 ) ) ;
#12250 = CARTESIAN_POINT ( 'NONE',  ( 20.39749770046332955, -9.194721705386330157, 1.203713204382251600 ) ) ;
#12251 = VERTEX_POINT ( 'NONE', #15406 ) ;
#12252 = CARTESIAN_POINT ( 'NONE',  ( -1.767766952966000060, 30.50000000000000000, 1.767766952966000060 ) ) ;
#12253 = VECTOR ( 'NONE', #19847, 1000.000000000000227 ) ;
#12254 = CARTESIAN_POINT ( 'NONE',  ( 11.55284350197085885, -9.059841367792975220, 9.307687628814361958 ) ) ;
#12255 = VECTOR ( 'NONE', #10460, 1000.000000000000114 ) ;
#12256 = VERTEX_POINT ( 'NONE', #4045 ) ;
#12257 = CARTESIAN_POINT ( 'NONE',  ( -2.535357900355000194, 24.74337675623999999, -0.2234184053773999867 ) ) ;
#12258 = CARTESIAN_POINT ( 'NONE',  ( 4.816292305294004983, 14.93029986592002345, 3.795759443924001442 ) ) ;
#12259 = CARTESIAN_POINT ( 'NONE',  ( 6.220855133530989178, 13.78415744763224815, -1.220025851734428901 ) ) ;
#12260 = CARTESIAN_POINT ( 'NONE',  ( -14.25243324638999809, -6.216878364870000340, -12.50000000000000000 ) ) ;
#12261 = CARTESIAN_POINT ( 'NONE',  ( 0.000000000000000000, 12.37689379448999993, 0.000000000000000000 ) ) ;
#12262 = CIRCLE ( 'NONE', #1023, 2.399999999999999911 ) ;
#12263 = ORIENTED_EDGE ( 'NONE', *, *, #23322, .F. ) ;
#12264 = CARTESIAN_POINT ( 'NONE',  ( -3.145406728938545893, 29.89685207198635553, -2.802800731853388960 ) ) ;
#12265 = DIRECTION ( 'NONE',  ( 0.000000000000000000, -1.000000000000000000, 0.000000000000000000 ) ) ;
#12266 = CARTESIAN_POINT ( 'NONE',  ( -4.000000000000056843, 24.75094615492120553, 2.107036910272268582 ) ) ;
#12267 = ORIENTED_EDGE ( 'NONE', *, *, #20319, .T. ) ;
#12268 = CARTESIAN_POINT ( 'NONE',  ( -19.11937752606000274, -10.08460061511999939, 1.755720681344000056 ) ) ;
#12269 = AXIS2_PLACEMENT_3D ( 'NONE', #12519, #8640, #4772 ) ;
#12270 = CARTESIAN_POINT ( 'NONE',  ( 23.99478584078000054, 6.383504859171999612, -12.40379814865999997 ) ) ;
#12271 = CARTESIAN_POINT ( 'NONE',  ( 14.88923352241194031, 10.28052023608410792, -1.022339429599108618 ) ) ;
#12272 = DIRECTION ( 'NONE',  ( -1.000000000000000000, 0.000000000000000000, -0.000000000000000000 ) ) ;
#12273 = CARTESIAN_POINT ( 'NONE',  ( 1.672509921849822945, 24.50639765414753768, 3.652834497693414839 ) ) ;
#12274 = CARTESIAN_POINT ( 'NONE',  ( 13.58272190881292474, 6.554870883473079779, -6.201906958780953438 ) ) ;
#12275 = CARTESIAN_POINT ( 'NONE',  ( 4.721753426476999138, 12.53551098956998544, 0.1045195479194000188 ) ) ;
#12276 = VERTEX_POINT ( 'NONE', #515 ) ;
#12277 = CARTESIAN_POINT ( 'NONE',  ( -24.18402430578868945, -7.007993001692642387, -7.183753820344653818 ) ) ;
#12278 = CARTESIAN_POINT ( 'NONE',  ( -1.619012473651841422, 29.49616192514975666, 1.435411994078731990 ) ) ;
#12279 = ORIENTED_EDGE ( 'NONE', *, *, #1258, .T. ) ;
#12280 = CARTESIAN_POINT ( 'NONE',  ( 23.99062354302999722, 6.216878364870000340, 12.50000000000000000 ) ) ;
#12281 = CARTESIAN_POINT ( 'NONE',  ( -16.83602692597334638, 9.825331796457355438, -3.486094970374975510 ) ) ;
#12282 = ORIENTED_EDGE ( 'NONE', *, *, #12322, .T. ) ;
#12283 = LINE ( 'NONE', #19673, #19581 ) ;
#12284 = CARTESIAN_POINT ( 'NONE',  ( 5.843331730810001901, 14.13764455460000136, -1.695804390486001401 ) ) ;
#12285 = CARTESIAN_POINT ( 'NONE',  ( 12.00000000000000178, -3.594391383428954700, -8.228416206764714858 ) ) ;
#12286 = CONICAL_SURFACE ( 'NONE', #3001, 13.23032192316000000, 1.235249617460683957 ) ;
#12287 = CARTESIAN_POINT ( 'NONE',  ( 14.15175919596000043, 0.2590669823852999598, -11.00306018672999997 ) ) ;
#12288 = CARTESIAN_POINT ( 'NONE',  ( 16.49081408530999937, 8.848325411959001130, 5.124349347825999601 ) ) ;
#12289 = EDGE_LOOP ( 'NONE', ( #17289, #6121, #20738, #6692, #12660, #16174, #230, #8186, #20668 ) ) ;
#12290 = CARTESIAN_POINT ( 'NONE',  ( -10.11278399292000074, 14.51541005890999969, 0.2520496489101999860 ) ) ;
#12291 = DIRECTION ( 'NONE',  ( 0.7071067811881966980, 0.7071067811848966711, 4.825990873454977813E-08 ) ) ;
#12292 =( LENGTH_UNIT ( ) NAMED_UNIT ( * ) SI_UNIT ( .MILLI., .METRE. ) );
#12293 = EDGE_LOOP ( 'NONE', ( #13569, #22528, #5287, #22418, #22559, #22885 ) ) ;
#12294 = CARTESIAN_POINT ( 'NONE',  ( 0.000000000000000000, -1.550000000000000044, 0.000000000000000000 ) ) ;
#12295 = CARTESIAN_POINT ( 'NONE',  ( 2.500000000000000000, 28.63419673618999894, 0.000000000000000000 ) ) ;
#12296 = CARTESIAN_POINT ( 'NONE',  ( 0.000000000000000000, 9.000000000000000000, 0.000000000000000000 ) ) ;
#12297 = CARTESIAN_POINT ( 'NONE',  ( -10.90000000000000036, 7.100000000000000533, 0.000000000000000000 ) ) ;
#12298 = CARTESIAN_POINT ( 'NONE',  ( 17.36346904825625259, -6.105277895300214475, 8.468900842036610754 ) ) ;
#12299 = AXIS2_PLACEMENT_3D ( 'NONE', #17033, #11596, #2025 ) ;
#12300 = CARTESIAN_POINT ( 'NONE',  ( -19.20653743917332434, 9.164159317821958695, 1.199712597205233600 ) ) ;
#12301 = DIRECTION ( 'NONE',  ( 1.000000000000000000, 0.000000000000000000, 0.000000000000000000 ) ) ;
#12302 = CARTESIAN_POINT ( 'NONE',  ( -4.306867197362858946, 13.60612586508986688, -4.963187192049142382 ) ) ;
#12303 = CARTESIAN_POINT ( 'NONE',  ( -1.631621777345116708, 30.11277217328136402, -1.415534461727001814 ) ) ;
#12304 = VERTEX_POINT ( 'NONE', #11675 ) ;
#12305 = CARTESIAN_POINT ( 'NONE',  ( -24.41513307468991201, -2.047838742126371958, 12.49997210310724327 ) ) ;
#12306 = CARTESIAN_POINT ( 'NONE',  ( 20.22702460548000047, -1.851192937421999751, 10.15609432501999976 ) ) ;
#12307 = CARTESIAN_POINT ( 'NONE',  ( 23.16496088167180645, -10.13946258324673444, -3.077221131437410495 ) ) ;
#12308 = CARTESIAN_POINT ( 'NONE',  ( -1.391452274478730544, 23.61431841429077494, -1.593469617572546682 ) ) ;
#12309 = ORIENTED_EDGE ( 'NONE', *, *, #21686, .F. ) ;
#12310 = EDGE_CURVE ( 'NONE', #1169, #9922, #19326, .T. ) ;
#12311 = CARTESIAN_POINT ( 'NONE',  ( -10.34021276376999943, 1.351277883783999990E-14, 0.000000000000000000 ) ) ;
#12312 = CARTESIAN_POINT ( 'NONE',  ( 4.852688899486731877, 14.56075982391421597, 3.781543657204870623 ) ) ;
#12313 = VECTOR ( 'NONE', #19342, 1000.000000000000000 ) ;
#12314 = CARTESIAN_POINT ( 'NONE',  ( 3.260899927695999345, 11.89447923387001183, -3.718744492640997379 ) ) ;
#12315 = VERTEX_POINT ( 'NONE', #2221 ) ;
#12316 = CARTESIAN_POINT ( 'NONE',  ( -14.89323719649020283, 8.655513120188558673, -5.700961162800999737 ) ) ;
#12317 = DIRECTION ( 'NONE',  ( -1.000000000000000000, 0.000000000000000000, 0.000000000000000000 ) ) ;
#12318 = ORIENTED_EDGE ( 'NONE', *, *, #17065, .F. ) ;
#12319 = DIRECTION ( 'NONE',  ( -0.000000000000000000, 1.000000000000000000, -0.000000000000000000 ) ) ;
#12320 = AXIS2_PLACEMENT_3D ( 'NONE', #20423, #19866, #5525 ) ;
#12321 = DIRECTION ( 'NONE',  ( 0.000000000000000000, 1.000000000000000000, 0.000000000000000000 ) ) ;
#12322 = EDGE_CURVE ( 'NONE', #8075, #6193, #20822, .T. ) ;
#12323 = ORIENTED_EDGE ( 'NONE', *, *, #22280, .F. ) ;
#12324 = CARTESIAN_POINT ( 'NONE',  ( 0.000000000000000000, 0.000000000000000000, 0.000000000000000000 ) ) ;
#12325 = CIRCLE ( 'NONE', #21612, 4.000000000000000000 ) ;
#12326 = CARTESIAN_POINT ( 'NONE',  ( 12.89756424930999934, 10.41448860350999972, -2.177620798092000598 ) ) ;
#12327 = CARTESIAN_POINT ( 'NONE',  ( -25.02706704405999716, 5.409545006709000070, -8.044608227789000310 ) ) ;
#12328 = CARTESIAN_POINT ( 'NONE',  ( -15.08585287682999976, 4.592917106262999205, 9.171186875826000673 ) ) ;
#12329 = DIRECTION ( 'NONE',  ( 0.000000000000000000, -1.000000000000000000, 0.000000000000000000 ) ) ;
#12330 = CARTESIAN_POINT ( 'NONE',  ( 19.93312451746000136, -5.235254289062000410, 7.414295425348999657 ) ) ;
#12331 = CARTESIAN_POINT ( 'NONE',  ( -4.000000000000000888, 26.43562577624027554, -1.040161751118715117 ) ) ;
#12332 = AXIS2_PLACEMENT_3D ( 'NONE', #21699, #6912, #10556 ) ;
#12333 = FACE_OUTER_BOUND ( 'NONE', #1375, .T. ) ;
#12334 = CARTESIAN_POINT ( 'NONE',  ( 14.89795833333333164, -7.239947641283004387, -5.563765923746745834 ) ) ;
#12335 = VERTEX_POINT ( 'NONE', #7916 ) ;
#12336 = CARTESIAN_POINT ( 'NONE',  ( 23.93192965267665073, -8.373336412066850087, 4.179851967670701107 ) ) ;
#12337 = CARTESIAN_POINT ( 'NONE',  ( -2.320455940937359962, 13.95415153313363454, 5.669042681536121897 ) ) ;
#12338 = CARTESIAN_POINT ( 'NONE',  ( -0.2419425476019000099, 26.86163313895000115, -2.456483904114000083 ) ) ;
#12339 = CARTESIAN_POINT ( 'NONE',  ( 3.025523437588009568, 26.41693820796410463, 2.872015382385962656 ) ) ;
#12340 = AXIS2_PLACEMENT_3D ( 'NONE', #10667, #23728, #18055 ) ;
#12341 = EDGE_CURVE ( 'NONE', #21964, #8871, #9368, .T. ) ;
#12342 = CARTESIAN_POINT ( 'NONE',  ( -20.41143800761999927, 10.68499263730999971, 2.863133627322999697 ) ) ;
#12343 = AXIS2_PLACEMENT_3D ( 'NONE', #7972, #17294, #1061 ) ;
#12344 =( GEOMETRIC_REPRESENTATION_CONTEXT ( 3 ) GLOBAL_UNCERTAINTY_ASSIGNED_CONTEXT ( ( #20100 ) ) GLOBAL_UNIT_ASSIGNED_CONTEXT ( ( #6831, #23544, #3455 ) ) REPRESENTATION_CONTEXT ( 'NONE', 'WORKASPACE' ) );
#12345 = CARTESIAN_POINT ( 'NONE',  ( -4.359756007405287903, 12.27018733399866868, 2.109445806361383013 ) ) ;
#12346 = VERTEX_POINT ( 'NONE', #19792 ) ;
#12347 = CARTESIAN_POINT ( 'NONE',  ( 0.000000000000000000, 16.89999999999999858, 0.000000000000000000 ) ) ;
#12348 = CARTESIAN_POINT ( 'NONE',  ( -24.50000000000453682, -0.2564718131638233367, -12.50000000000233946 ) ) ;
#12349 = CARTESIAN_POINT ( 'NONE',  ( -10.64039927319732826, 15.44563189339511133, 1.499887593842308853 ) ) ;
#12350 = CIRCLE ( 'NONE', #9617, 12.50000000000000533 ) ;
#12351 = CARTESIAN_POINT ( 'NONE',  ( -1.103611694251628084, 30.16587371767807824, 1.992807635840708302 ) ) ;
#12352 = ADVANCED_FACE ( 'NONE', ( #5251 ), #16164, .F. ) ;
#12353 = DIRECTION ( 'NONE',  ( 0.000000000000000000, 0.000000000000000000, -1.000000000000000000 ) ) ;
#12354 = CARTESIAN_POINT ( 'NONE',  ( -16.28651788626999775, 5.579994563924000062, 9.896790535726999849 ) ) ;
#12355 = CARTESIAN_POINT ( 'NONE',  ( 17.56125142131000061, 3.538711643716999866, -9.078802261343000168 ) ) ;
#12356 = CARTESIAN_POINT ( 'NONE',  ( 18.49749537389288179, 10.29274632983991289, -1.665592463132857137 ) ) ;
#12357 = CONICAL_SURFACE ( 'NONE', #1902, 9.136555860486998526, 0.02565634000431304615 ) ;
#12358 = ORIENTED_EDGE ( 'NONE', *, *, #19645, .T. ) ;
#12359 = CARTESIAN_POINT ( 'NONE',  ( 2.500000000000000000, 28.41666666666666430, -0.3272492347489370235 ) ) ;
#12360 = CARTESIAN_POINT ( 'NONE',  ( 2.675621865512000319, 29.28399530016000085, -0.5102467047576000336 ) ) ;
#12361 = DIRECTION ( 'NONE',  ( 0.000000000000000000, 0.000000000000000000, -1.000000000000000000 ) ) ;
#12362 = CARTESIAN_POINT ( 'NONE',  ( -2.129837485869429337, 13.91293410602873415, -5.743800140878768445 ) ) ;
#12363 = AXIS2_PLACEMENT_3D ( 'NONE', #13168, #15333, #7961 ) ;
#12364 = ORIENTED_EDGE ( 'NONE', *, *, #14673, .T. ) ;
#12365 = EDGE_CURVE ( 'NONE', #3930, #8569, #16488, .T. ) ;
#12366 = LINE ( 'NONE', #19753, #8723 ) ;
#12367 = CARTESIAN_POINT ( 'NONE',  ( -24.41513307469365657, 11.84921275893194093, -4.476505678047745462 ) ) ;
#12368 = LINE ( 'NONE', #14721, #3040 ) ;
#12369 = PLANE ( 'NONE',  #9647 ) ;
#12370 = CARTESIAN_POINT ( 'NONE',  ( 16.65020012662924742, 9.567642578645610740, 4.135108216434137951 ) ) ;
#12371 = CARTESIAN_POINT ( 'NONE',  ( -3.834781054353642027, 14.03942942280233552, 4.850192126058685993 ) ) ;
#12372 = CARTESIAN_POINT ( 'NONE',  ( -4.915212978806001054, 12.43953049402999511, 0.1288957748261999048 ) ) ;
#12373 = ADVANCED_FACE ( 'NONE', ( #18321 ), #1494, .T. ) ;
#12374 = DIRECTION ( 'NONE',  ( 1.000000000000000000, 0.000000000000000000, 0.000000000000000000 ) ) ;
#12375 = ORIENTED_EDGE ( 'NONE', *, *, #17739, .T. ) ;
#12376 = CARTESIAN_POINT ( 'NONE',  ( 18.93264468355999952, 0.000000000000000000, 0.000000000000000000 ) ) ;
#12377 = EDGE_CURVE ( 'NONE', #5826, #19902, #3344, .T. ) ;
#12378 = CARTESIAN_POINT ( 'NONE',  ( 2.500000000000000000, 27.83419673618999823, 0.000000000000000000 ) ) ;
#12379 = VERTEX_POINT ( 'NONE', #14785 ) ;
#12380 = CIRCLE ( 'NONE', #9268, 2.399999999999999911 ) ;
#12381 = CARTESIAN_POINT ( 'NONE',  ( -2.550975086816000381, 24.01276803249999858, -0.9922851024814999255 ) ) ;
#12382 = CYLINDRICAL_SURFACE ( 'NONE', #3569, 12.44999999999999929 ) ;
#12383 = CARTESIAN_POINT ( 'NONE',  ( -2.915062434927890855, 13.09062905184296355, 6.080193266496893401 ) ) ;
#12384 = AXIS2_PLACEMENT_3D ( 'NONE', #9398, #3598, #16661 ) ;
#12385 = PLANE ( 'NONE',  #21550 ) ;
#12386 = DIRECTION ( 'NONE',  ( 0.000000000000000000, 1.000000000000000000, 0.000000000000000000 ) ) ;
#12387 = DIRECTION ( 'NONE',  ( 0.000000000000000000, 1.000000000000000000, 0.000000000000000000 ) ) ;
#12388 = ADVANCED_FACE ( 'NONE', ( #7167, #3321 ), #21726, .F. ) ;
#12389 = VERTEX_POINT ( 'NONE', #1615 ) ;
#12390 = EDGE_CURVE ( 'NONE', #16342, #20086, #12407, .T. ) ;
#12391 = CARTESIAN_POINT ( 'NONE',  ( -8.000000000000000000, -9.651424765286998664, 0.000000000000000000 ) ) ;
#12392 = FACE_OUTER_BOUND ( 'NONE', #11021, .T. ) ;
#12393 = DIRECTION ( 'NONE',  ( 0.000000000000000000, 0.5000000000000169864, -0.8660254037844288266 ) ) ;
#12394 = VERTEX_POINT ( 'NONE', #7283 ) ;
#12395 = CARTESIAN_POINT ( 'NONE',  ( -23.34642367104000016, 6.759604227058999548, 8.376683203238998843 ) ) ;
#12396 = CARTESIAN_POINT ( 'NONE',  ( 20.15099999999999980, -9.188396088570998543, 0.000000000000000000 ) ) ;
#12397 = CARTESIAN_POINT ( 'NONE',  ( 15.05994471934696222, 9.084270234149091294, 4.927946041152025280 ) ) ;
#12398 = DIRECTION ( 'NONE',  ( 0.000000000000000000, 1.000000000000000000, 0.000000000000000000 ) ) ;
#12399 = CARTESIAN_POINT ( 'NONE',  ( 1.699986957659999964, 9.000014576061998284, -0.8485216275457999613 ) ) ;
#12400 = CARTESIAN_POINT ( 'NONE',  ( -23.13201460959644606, 9.263705172255090048, 1.213526924431011178 ) ) ;
#12401 = CARTESIAN_POINT ( 'NONE',  ( -4.287094022045000230, 12.36933742260000280, -1.995563538544997240 ) ) ;
#12402 = ORIENTED_EDGE ( 'NONE', *, *, #18866, .F. ) ;
#12403 = CARTESIAN_POINT ( 'NONE',  ( -1.852637453037785153, 26.30370469418262047, 1.202693574547283983 ) ) ;
#12404 = CARTESIAN_POINT ( 'NONE',  ( -0.2347037422651374605, 29.21777112581033364, -2.147026567374833661 ) ) ;
#12405 = EDGE_LOOP ( 'NONE', ( #14768, #23469, #21082, #17246 ) ) ;
#12406 = DIRECTION ( 'NONE',  ( 0.000000000000000000, 0.000000000000000000, 1.000000000000000000 ) ) ;
#12407 = LINE ( 'NONE', #17971, #10393 ) ;
#12408 = VECTOR ( 'NONE', #17285, 1000.000000000000000 ) ;
#12409 = ORIENTED_EDGE ( 'NONE', *, *, #12057, .F. ) ;
#12410 = CARTESIAN_POINT ( 'NONE',  ( -2.000000000000000000, 30.00000000000000000, -3.464101615137999968 ) ) ;
#12411 = CARTESIAN_POINT ( 'NONE',  ( 0.2857557581101721755, 30.80642105250836238, -2.193578937681244678 ) ) ;
#12412 = CARTESIAN_POINT ( 'NONE',  ( 12.00000000000000533, 3.282172266231635493, -8.358364226753291604 ) ) ;
#12413 = CARTESIAN_POINT ( 'NONE',  ( 0.000000000000000000, 15.00000000000000000, 0.000000000000000000 ) ) ;
#12414 = CARTESIAN_POINT ( 'NONE',  ( 12.43237658531000100, 5.753414546153999609, -8.323445001914000940 ) ) ;
#12415 = ADVANCED_FACE ( 'NONE', ( #3202 ), #14557, .T. ) ;
#12416 = ORIENTED_EDGE ( 'NONE', *, *, #12950, .F. ) ;
#12417 = CARTESIAN_POINT ( 'NONE',  ( -5.194121241777001075, 12.44999999999999929, 0.000000000000000000 ) ) ;
#12418 = CARTESIAN_POINT ( 'NONE',  ( 13.50000000000000000, 9.050782136005169676, -2.623848385460896271 ) ) ;
#12419 = CARTESIAN_POINT ( 'NONE',  ( 21.05799999999999983, 9.211671496174000495, 0.000000000000000000 ) ) ;
#12420 = VERTEX_POINT ( 'NONE', #8765 ) ;
#12421 = CARTESIAN_POINT ( 'NONE',  ( 11.53663804754501321, 9.092401935531025714, 9.251313393131750829 ) ) ;
#12422 = CARTESIAN_POINT ( 'NONE',  ( 22.35284124051811716, 2.717056027886565417, 10.21878362023675635 ) ) ;
#12423 = CARTESIAN_POINT ( 'NONE',  ( -14.00000000000000178, 5.842258123726868035, 7.306472440924601131 ) ) ;
#12424 = CARTESIAN_POINT ( 'NONE',  ( 16.27435937805609356, -0.08560440561706507412, -10.36554760290414734 ) ) ;
#12425 = CARTESIAN_POINT ( 'NONE',  ( -18.41291243917333631, -8.905853451295076439, 2.393251276420213181 ) ) ;
#12426 = CARTESIAN_POINT ( 'NONE',  ( 2.243942538766000361, 29.77722651399999876, 0.6739745749383999618 ) ) ;
#12427 = CIRCLE ( 'NONE', #1968, 0.1000000000000003525 ) ;
#12428 = B_SPLINE_CURVE_WITH_KNOTS ( 'NONE', 3,
 ( #16819, #3641, #5686, #2169, #3993, #5573 ),
 .UNSPECIFIED., .F., .F.,
 ( 4, 1, 1, 4 ),
 ( 0.000000000000000000, 0.3333333333333000081, 0.6666666666667000474, 1.000000000000000000 ),
 .UNSPECIFIED. ) ;
#12429 = DIRECTION ( 'NONE',  ( -0.9996708941621516020, 0.02565352539211874019, 0.000000000000000000 ) ) ;
#12430 = CARTESIAN_POINT ( 'NONE',  ( 0.4219218820329893593, 29.97882480414182638, -2.122083357744672494 ) ) ;
#12431 = ORIENTED_EDGE ( 'NONE', *, *, #6587, .F. ) ;
#12432 = CARTESIAN_POINT ( 'NONE',  ( 23.23091206975999867, -5.927610222709999377, -9.828413730229001999 ) ) ;
#12433 = CARTESIAN_POINT ( 'NONE',  ( 23.10821411434546846, -10.53956942713338485, -1.043342762108328881 ) ) ;
#12434 = DIRECTION ( 'NONE',  ( 0.000000000000000000, 0.9899013191676121481, -0.1417581684074016302 ) ) ;
#12435 = VERTEX_POINT ( 'NONE', #6942 ) ;
#12436 = CARTESIAN_POINT ( 'NONE',  ( 23.99062354302999722, -7.716878364870000340, -11.63397459621999985 ) ) ;
#12437 = CARTESIAN_POINT ( 'NONE',  ( -5.425547005761002239, 14.33167101788998110, 5.123586822884999670 ) ) ;
#12438 = CARTESIAN_POINT ( 'NONE',  ( -4.656229534563997241, 12.40715657742001454, -1.679150298895001114 ) ) ;
#12439 = ORIENTED_EDGE ( 'NONE', *, *, #19335, .T. ) ;
#12440 = DIRECTION ( 'NONE',  ( 0.000000000000000000, 0.000000000000000000, 1.000000000000000000 ) ) ;
#12441 = ORIENTED_EDGE ( 'NONE', *, *, #18014, .T. ) ;
#12442 = DIRECTION ( 'NONE',  ( 0.000000000000000000, 1.000000000000000000, 0.000000000000000000 ) ) ;
#12443 = PRODUCT_CONTEXT ( 'NONE', #4320, 'mechanical' ) ;
#12444 = CARTESIAN_POINT ( 'NONE',  ( 11.50000000000000000, 7.000000000000000000, 0.000000000000000000 ) ) ;
#12445 = EDGE_LOOP ( 'NONE', ( #23378, #22588, #23273 ) ) ;
#12446 = CARTESIAN_POINT ( 'NONE',  ( -10.04281598261999875, 16.38798294977999959, -1.000000000000000000 ) ) ;
#12447 = CARTESIAN_POINT ( 'NONE',  ( -12.28892333464999886, 12.23011958036999935, -9.372058967585999767 ) ) ;
#12448 = CARTESIAN_POINT ( 'NONE',  ( -25.07905962863999960, -4.825123054982000781, -8.416491615424000372 ) ) ;
#12449 = EDGE_CURVE ( 'NONE', #18916, #23321, #21950, .T. ) ;
#12450 = CARTESIAN_POINT ( 'NONE',  ( -14.41041139552000061, -8.718623938206999213, 6.329101201815000799 ) ) ;
#12451 = FACE_OUTER_BOUND ( 'NONE', #22212, .T. ) ;
#12452 = CARTESIAN_POINT ( 'NONE',  ( -24.08723349875008068, 10.05054684006879917, -3.366032446606162853 ) ) ;
#12453 = CARTESIAN_POINT ( 'NONE',  ( 2.172046235086991128, 27.39994352002885236, 0.07647517823428454098 ) ) ;
#12454 = DIRECTION ( 'NONE',  ( 0.000000000000000000, 1.000000000000000000, 0.000000000000000000 ) ) ;
#12455 = CARTESIAN_POINT ( 'NONE',  ( 24.28255857085268943, -8.769700062105057370, 9.810433925293667201 ) ) ;
#12456 = ORIENTED_EDGE ( 'NONE', *, *, #21817, .F. ) ;
#12457 = CARTESIAN_POINT ( 'NONE',  ( 23.24497483482962679, 8.949111925071910889, 2.821285790844791475 ) ) ;
#12458 = CARTESIAN_POINT ( 'NONE',  ( 3.157813948402969473, 14.17377548709831814, 5.253260371035572085 ) ) ;
#12459 = CARTESIAN_POINT ( 'NONE',  ( 0.04846321314153999998, 27.25163313894999817, 2.467893978438000069 ) ) ;
#12460 = CARTESIAN_POINT ( 'NONE',  ( -20.74560709917999901, 6.919428769260999701, -8.642269477009000056 ) ) ;
#12461 = CARTESIAN_POINT ( 'NONE',  ( -4.280167514080574165, 12.24264458569462732, 2.262784844200641743 ) ) ;
#12462 = ORIENTED_EDGE ( 'NONE', *, *, #1828, .T. ) ;
#12463 = DIRECTION ( 'NONE',  ( 0.000000000000000000, -1.000000000000000000, 0.000000000000000000 ) ) ;
#12464 = CARTESIAN_POINT ( 'NONE',  ( 4.423996544771463313, 12.29285732557641708, -1.971860468088503016 ) ) ;
#12465 = CARTESIAN_POINT ( 'NONE',  ( 24.11388506871679738, -1.064351356577731833, -9.431612009895189885 ) ) ;
#12466 = DIRECTION ( 'NONE',  ( -1.000000000000000000, 0.000000000000000000, 0.000000000000000000 ) ) ;
#12467 = ORIENTED_EDGE ( 'NONE', *, *, #18579, .T. ) ;
#12468 = DIRECTION ( 'NONE',  ( 0.000000000000000000, 1.000000000000000000, 0.000000000000000000 ) ) ;
#12469 = CARTESIAN_POINT ( 'NONE',  ( -15.27086614641999951, -1.548365329537000123, -11.22688807791999999 ) ) ;
#12470 = CARTESIAN_POINT ( 'NONE',  ( 12.62531392131000096, 8.177682633693001080, 5.055777280222000236 ) ) ;
#12471 = CARTESIAN_POINT ( 'NONE',  ( 18.60941832878186020, 10.17571512187342719, 2.300618295382859113 ) ) ;
#12472 = ADVANCED_FACE ( 'NONE', ( #19905 ), #5138, .T. ) ;
#12473 = VERTEX_POINT ( 'NONE', #10826 ) ;
#12474 = CARTESIAN_POINT ( 'NONE',  ( -22.87210175995843642, 9.258583067823760615, -6.329161777784410158E-06 ) ) ;
#12475 = CARTESIAN_POINT ( 'NONE',  ( -2.156765450510000015, 30.19818128708999794, -0.9123105095192000080 ) ) ;
#12476 = DIRECTION ( 'NONE',  ( -1.000000000000000000, 0.000000000000000000, 0.000000000000000000 ) ) ;
#12477 = CARTESIAN_POINT ( 'NONE',  ( 13.50000000000000178, -9.667143133194834093, 1.150750041508975974 ) ) ;
#12478 = AXIS2_PLACEMENT_3D ( 'NONE', #3185, #23637, #7150 ) ;
#12479 = EDGE_LOOP ( 'NONE', ( #18621, #4690, #10726, #14121, #18323, #23429, #21752, #2640, #19263, #11924, #16876 ) ) ;
#12480 = CARTESIAN_POINT ( 'NONE',  ( 18.75008227645999881, 0.000000000000000000, 0.000000000000000000 ) ) ;
#12481 = DIRECTION ( 'NONE',  ( 0.000000000000000000, 1.000000000000000000, 0.000000000000000000 ) ) ;
#12482 = DIRECTION ( 'NONE',  ( 0.000000000000000000, -1.000000000000000000, 0.000000000000000000 ) ) ;
#12483 = CARTESIAN_POINT ( 'NONE',  ( -23.76509227919060407, -8.602129290516417726, 4.230010080241071613 ) ) ;
#12484 = CARTESIAN_POINT ( 'NONE',  ( 14.14125231517192383, -4.302439909528064987, -9.420726477911008701 ) ) ;
#12485 = CARTESIAN_POINT ( 'NONE',  ( 24.50000000000000000, -10.82531754731000007, 6.250000000000000000 ) ) ;
#12486 = CARTESIAN_POINT ( 'NONE',  ( 2.372479547917001330, 11.76473980360000837, 4.356678035347999689 ) ) ;
#12487 = EDGE_CURVE ( 'NONE', #568, #14317, #9603, .T. ) ;
#12488 = CARTESIAN_POINT ( 'NONE',  ( 2.500000000000000000, 30.23419673619000037, 0.000000000000000000 ) ) ;
#12489 = ORIENTED_EDGE ( 'NONE', *, *, #10127, .F. ) ;
#12490 = CARTESIAN_POINT ( 'NONE',  ( 0.000000000000000000, -10.00000000000000000, 0.000000000000000000 ) ) ;
#12491 = CARTESIAN_POINT ( 'NONE',  ( 0.1752525089982897022, 24.75094615491968852, -4.517620070270786492 ) ) ;
#12492 = ORIENTED_EDGE ( 'NONE', *, *, #13472, .F. ) ;
#12493 = CARTESIAN_POINT ( 'NONE',  ( 1.848971201200000136, 25.85810122863999894, 1.749110969876999988 ) ) ;
#12494 = FACE_OUTER_BOUND ( 'NONE', #22207, .T. ) ;
#12495 = CARTESIAN_POINT ( 'NONE',  ( -19.42565315260486614, -9.827978956737730698, 3.502397672827030739 ) ) ;
#12496 = DIRECTION ( 'NONE',  ( 0.000000000000000000, 0.000000000000000000, -1.000000000000000000 ) ) ;
#12497 = CARTESIAN_POINT ( 'NONE',  ( -5.694829656253005190, 15.68676470074999685, -2.067368767709001798 ) ) ;
#12498 = EDGE_CURVE ( 'NONE', #18819, #4661, #7597, .T. ) ;
#12499 = CARTESIAN_POINT ( 'NONE',  ( 1.709999999999999964, 9.000000000000000000, 0.3720215047547999476 ) ) ;
#12500 = ORIENTED_EDGE ( 'NONE', *, *, #18250, .F. ) ;
#12501 = CARTESIAN_POINT ( 'NONE',  ( -3.025523437588010012, 29.91693820796410108, -2.872015382385962656 ) ) ;
#12502 = CARTESIAN_POINT ( 'NONE',  ( -1.973459554958962414, 26.24813749873406010, 0.8485066749672629527 ) ) ;
#12503 = DIRECTION ( 'NONE',  ( -0.9996708941621507138, -0.02565352539215873945, -1.663606736649919489E-14 ) ) ;
#12504 = EDGE_CURVE ( 'NONE', #20964, #11498, #21986, .T. ) ;
#12505 = ORIENTED_EDGE ( 'NONE', *, *, #22074, .F. ) ;
#12506 = CARTESIAN_POINT ( 'NONE',  ( -19.74772222328000026, 7.504538301275000656, 7.579212376565000575 ) ) ;
#12507 = FACE_OUTER_BOUND ( 'NONE', #9583, .T. ) ;
#12508 = CARTESIAN_POINT ( 'NONE',  ( 15.14946676811930892, 7.172451777050300237, 7.444582818315895523 ) ) ;
#12509 = LINE ( 'NONE', #21597, #12178 ) ;
#12510 = CARTESIAN_POINT ( 'NONE',  ( 24.30943970833000023, -6.839077597037000800, 9.006887850905000548 ) ) ;
#12511 = CARTESIAN_POINT ( 'NONE',  ( -3.000000000000000000, 19.09999999999999787, 0.000000000000000000 ) ) ;
#12512 = CARTESIAN_POINT ( 'NONE',  ( -22.58373927040480211, -4.100154767907044473, 8.316095026788374867 ) ) ;
#12513 = CARTESIAN_POINT ( 'NONE',  ( 4.436770113162001650, 12.42462873132999057, -1.662129547883000047 ) ) ;
#12514 = ORIENTED_EDGE ( 'NONE', *, *, #10576, .F. ) ;
#12515 = ORIENTED_EDGE ( 'NONE', *, *, #3366, .T. ) ;
#12516 = DIRECTION ( 'NONE',  ( 0.000000000000000000, 0.7071067811866525998, -0.7071067811864425456 ) ) ;
#12517 = EDGE_CURVE ( 'NONE', #15215, #17884, #23478, .T. ) ;
#12518 = ORIENTED_EDGE ( 'NONE', *, *, #21424, .F. ) ;
#12519 = CARTESIAN_POINT ( 'NONE',  ( 0.000000000000000000, 15.00000000000000000, 0.000000000000000000 ) ) ;
#12520 = CARTESIAN_POINT ( 'NONE',  ( 0.000000000000000000, -1.550000000000000044, 0.000000000000000000 ) ) ;
#12521 = ORIENTED_EDGE ( 'NONE', *, *, #491, .T. ) ;
#12522 = DIRECTION ( 'NONE',  ( 0.000000000000000000, 1.000000000000000000, 0.000000000000000000 ) ) ;
#12523 = CARTESIAN_POINT ( 'NONE',  ( 6.356497079780072168E-07, 30.81706029784504963, -2.183072574220335849 ) ) ;
#12524 = DIRECTION ( 'NONE',  ( 0.000000000000000000, 1.000000000000000000, 0.000000000000000000 ) ) ;
#12525 = CARTESIAN_POINT ( 'NONE',  ( 14.87356278734000092, 6.387809963882999931, 8.986984594874000365 ) ) ;
#12526 = ORIENTED_EDGE ( 'NONE', *, *, #1948, .T. ) ;
#12527 = CARTESIAN_POINT ( 'NONE',  ( -11.91164815959000123, 4.681446530594000066, -13.43333759439000019 ) ) ;
#12528 = CARTESIAN_POINT ( 'NONE',  ( 13.50000000000000000, 9.584206265642421840, 0.6392395819158175341 ) ) ;
#12529 = DIRECTION ( 'NONE',  ( 0.000000000000000000, 1.000000000000000000, 0.000000000000000000 ) ) ;
#12530 = EDGE_CURVE ( 'NONE', #2558, #16650, #7669, .T. ) ;
#12531 = VERTEX_POINT ( 'NONE', #22530 ) ;
#12532 = EDGE_CURVE ( 'NONE', #10909, #889, #5731, .T. ) ;
#12533 = CARTESIAN_POINT ( 'NONE',  ( 23.73532679364096154, 10.43134061897112552, -1.947531773972139835 ) ) ;
#12534 = AXIS2_PLACEMENT_3D ( 'NONE', #22573, #406, #22456 ) ;
#12535 = CARTESIAN_POINT ( 'NONE',  ( -10.90000000000000036, -10.59999999999999964, 0.000000000000000000 ) ) ;
#12536 = CARTESIAN_POINT ( 'NONE',  ( 17.60422380272236964, -10.38553041900061835, 1.163297858921190642 ) ) ;
#12537 = CARTESIAN_POINT ( 'NONE',  ( -17.90484265138000097, 4.662643172107000744, 10.07117353495000067 ) ) ;
#12538 = CARTESIAN_POINT ( 'NONE',  ( -14.33281102374373184, -13.40129170500426348, 1.788281879885561754 ) ) ;
#12539 = UNCERTAINTY_MEASURE_WITH_UNIT (LENGTH_MEASURE( 1.000000000000000082E-05 ), #21285, 'distance_accuracy_value', 'NONE');
#12540 = CARTESIAN_POINT ( 'NONE',  ( -17.38302573041000088, 5.218320932965999859, 8.277968099418000492 ) ) ;
#12541 = CARTESIAN_POINT ( 'NONE',  ( 1.679203100328423570, 29.89047614560958976, -1.358641863343548639 ) ) ;
#12542 = EDGE_CURVE ( 'NONE', #5263, #165, #15782, .T. ) ;
#12543 = ORIENTED_EDGE ( 'NONE', *, *, #6558, .F. ) ;
#12544 = CARTESIAN_POINT ( 'NONE',  ( 21.10515180059999807, -11.40348565785000012, 0.5907356610812999342 ) ) ;
#12545 = EDGE_CURVE ( 'NONE', #8305, #6675, #14626, .T. ) ;
#12546 = CARTESIAN_POINT ( 'NONE',  ( 24.44176314649520165, -0.04959099671479073879, 10.63117537983664107 ) ) ;
#12547 = CARTESIAN_POINT ( 'NONE',  ( 0.5500000000000000444, 1.217911241751999838E-14, 0.000000000000000000 ) ) ;
#12548 = AXIS2_PLACEMENT_3D ( 'NONE', #4676, #7410, #5717 ) ;
#12549 = ORIENTED_EDGE ( 'NONE', *, *, #11166, .F. ) ;
#12550 = CARTESIAN_POINT ( 'NONE',  ( 0.8007553318486925198, 23.87661134863360246, 2.106186139113426226 ) ) ;
#12551 = CARTESIAN_POINT ( 'NONE',  ( 4.921741273393275051, 14.32471902143299758, -3.831972585562755995 ) ) ;
#12552 = CARTESIAN_POINT ( 'NONE',  ( -4.833494752206995315, 12.42175356251998330, 0.1521745567910999519 ) ) ;
#12553 = ORIENTED_EDGE ( 'NONE', *, *, #18678, .F. ) ;
#12554 = CARTESIAN_POINT ( 'NONE',  ( 4.649999999999999467, 17.00000000000000000, 0.000000000000000000 ) ) ;
#12555 = VERTEX_POINT ( 'NONE', #20722 ) ;
#12556 = CARTESIAN_POINT ( 'NONE',  ( 0.9536831490418160584, 27.37231439908301311, -1.970019352804785795 ) ) ;
#12557 = DIRECTION ( 'NONE',  ( -0.7071067811880967779, 0.7071067811849969242, 4.142943916964978477E-08 ) ) ;
#12558 = VERTEX_POINT ( 'NONE', #4128 ) ;
#12559 = LINE ( 'NONE', #14131, #18632 ) ;
#12560 = CIRCLE ( 'NONE', #8704, 4.750000000000000000 ) ;
#12561 = CARTESIAN_POINT ( 'NONE',  ( -4.894724768791110847, 15.80180785695556267, -3.682445206660954540 ) ) ;
#12562 = CARTESIAN_POINT ( 'NONE',  ( -24.91847294367000032, 0.3645929728760000099, -10.20369181617000010 ) ) ;
#12563 = CARTESIAN_POINT ( 'NONE',  ( -16.16755505407000371, -1.332106624616000046, -9.660193477322000177 ) ) ;
#12564 = CARTESIAN_POINT ( 'NONE',  ( 19.09283333333333132, 8.004919495498239002, -4.613892360491747446 ) ) ;
#12565 = CARTESIAN_POINT ( 'NONE',  ( -23.08356359459203233, -10.56989946170757122, -0.1237766064311238562 ) ) ;
#12566 = CARTESIAN_POINT ( 'NONE',  ( -1.766837003731960287, 26.92292278627816415, -1.325251963590689197 ) ) ;
#12567 = FACE_OUTER_BOUND ( 'NONE', #12479, .T. ) ;
#12568 = CARTESIAN_POINT ( 'NONE',  ( 2.093630357446228718, 30.63581803265235592, -0.5390189978566096718 ) ) ;
#12569 = ORIENTED_EDGE ( 'NONE', *, *, #17943, .T. ) ;
#12570 = CARTESIAN_POINT ( 'NONE',  ( -61.30710721978000066, 16.31160201366999729, 2.000000000000000000 ) ) ;
#12571 = DIRECTION ( 'NONE',  ( 1.000000000000000000, 0.000000000000000000, 0.000000000000000000 ) ) ;
#12572 = CARTESIAN_POINT ( 'NONE',  ( 0.4339301335947999827, 26.47163313894999703, 2.429928970624000151 ) ) ;
#12573 = CARTESIAN_POINT ( 'NONE',  ( -24.36619054344396673, -4.196740350062569291, -9.738563182048725508 ) ) ;
#12574 = CARTESIAN_POINT ( 'NONE',  ( 1.906085653762000121, 28.06364211382000207, -1.273605814386999713 ) ) ;
#12575 = AXIS2_PLACEMENT_3D ( 'NONE', #6653, #21441, #10663 ) ;
#12576 = CARTESIAN_POINT ( 'NONE',  ( 3.929826322352642620, 12.12559072794920745, 2.830479342495737960 ) ) ;
#12577 = ORIENTED_EDGE ( 'NONE', *, *, #23928, .F. ) ;
#12578 = CARTESIAN_POINT ( 'NONE',  ( 18.29920833333331842, -9.140875464714465437, 1.196664747960662245 ) ) ;
#12579 = DIRECTION ( 'NONE',  ( 0.000000000000000000, -1.000000000000000000, 0.000000000000000000 ) ) ;
#12580 = DIRECTION ( 'NONE',  ( 1.000000000000000000, 0.000000000000000000, 0.000000000000000000 ) ) ;
#12581 = B_SPLINE_CURVE_WITH_KNOTS ( 'NONE', 3,
 ( #15463, #20927, #4333, #4455, #6262, #19225 ),
 .UNSPECIFIED., .F., .F.,
 ( 4, 2, 4 ),
 ( 0.000000000000000000, 0.1676274590533611553, 0.3352549181067223105 ),
 .UNSPECIFIED. ) ;
#12582 = B_SPLINE_CURVE_WITH_KNOTS ( 'NONE', 3,
 ( #9946, #2690, #7894, #2438, #8141, #8011 ),
 .UNSPECIFIED., .F., .F.,
 ( 4, 2, 4 ),
 ( 4.972458724030523193E-05, 0.0005957450933333919684, 0.001141765599426478820 ),
 .UNSPECIFIED. ) ;
#12583 = CARTESIAN_POINT ( 'NONE',  ( 11.91174123157076004, 2.862535089823035062, -8.618805975702651168 ) ) ;
#12584 = ORIENTED_EDGE ( 'NONE', *, *, #17943, .F. ) ;
#12585 = CARTESIAN_POINT ( 'NONE',  ( -1.536366799937239458, 24.11666666666666359, 1.999167105995485860 ) ) ;
#12586 = CARTESIAN_POINT ( 'NONE',  ( -16.29067920454665241, 2.379230875366821873, -8.852713068186144341 ) ) ;
#12587 = CARTESIAN_POINT ( 'NONE',  ( 12.18656392131000210, 5.460236994095999385, -7.899338765649998706 ) ) ;
#12588 = CARTESIAN_POINT ( 'NONE',  ( 18.71070319846496233, 8.742660180748359267, 5.685782510781925758 ) ) ;
#12589 = PRODUCT_DEFINITION_CONTEXT ( 'detailed design', #16691, 'design' ) ;
#12590 = ORIENTED_EDGE ( 'NONE', *, *, #208, .F. ) ;
#12591 = CARTESIAN_POINT ( 'NONE',  ( -24.49594166687865382, 0.5121745395634360598, 12.49996680834482454 ) ) ;
#12592 = CARTESIAN_POINT ( 'NONE',  ( 11.00000000000000000, -7.000000000000000000, 0.000000000000000000 ) ) ;
#12593 = CARTESIAN_POINT ( 'NONE',  ( -12.49650014189999858, 7.040626845934999878, -5.593302763177000259 ) ) ;
#12594 = CARTESIAN_POINT ( 'NONE',  ( 13.50000000000000000, -6.542208323345639620, 7.794097110268465300 ) ) ;
#12595 = CIRCLE ( 'NONE', #23398, 2.649999999999999911 ) ;
#12596 = ORIENTED_EDGE ( 'NONE', *, *, #12532, .T. ) ;
#12597 = DIRECTION ( 'NONE',  ( 0.000000000000000000, 1.000000000000000000, 0.000000000000000000 ) ) ;
#12598 = CARTESIAN_POINT ( 'NONE',  ( -14.25699038479000080, 13.93375672974000068, 0.000000000000000000 ) ) ;
#12599 = CARTESIAN_POINT ( 'NONE',  ( 2.402140947178999647E-14, 29.00000000000000000, 2.500000000000000000 ) ) ;
#12600 = CARTESIAN_POINT ( 'NONE',  ( 24.50000000000000355, -6.132195556898603073, 8.621549258802161830 ) ) ;
#12601 = CARTESIAN_POINT ( 'NONE',  ( 7.278495274186999708, 27.32666689084959799, -6.000000000000000000 ) ) ;
#12602 = CARTESIAN_POINT ( 'NONE',  ( -1.099366357925000148, 11.57595430713999818, 4.853237177371000577 ) ) ;
#12603 = CARTESIAN_POINT ( 'NONE',  ( -24.42716110443999966, -9.258832120292998624, -5.480706378555000313 ) ) ;
#12604 = ORIENTED_EDGE ( 'NONE', *, *, #2096, .T. ) ;
#12605 = CARTESIAN_POINT ( 'NONE',  ( -9.000000000000000000, 18.50000000000000000, -5.000000000000000000 ) ) ;
#12606 = CARTESIAN_POINT ( 'NONE',  ( -4.000000000000000000, 26.50000000000000711, 0.3708744353061897980 ) ) ;
#12607 = ORIENTED_EDGE ( 'NONE', *, *, #14737, .F. ) ;
#12608 = EDGE_CURVE ( 'NONE', #16051, #8097, #92, .T. ) ;
#12609 = CARTESIAN_POINT ( 'NONE',  ( 2.478485849303000421, 24.32535507907999772, 0.5788465350207999682 ) ) ;
#12610 = DIRECTION ( 'NONE',  ( -1.000000000000000000, 0.000000000000000000, 0.000000000000000000 ) ) ;
#12611 = CONICAL_SURFACE ( 'NONE', #12228, 2.154903751016000069, 0.7853981633972997312 ) ;
#12612 = CARTESIAN_POINT ( 'NONE',  ( -19.49229789055419459, -9.829589521208637493, 3.502971628430095130 ) ) ;
#12613 = CIRCLE ( 'NONE', #7557, 7.500000000000000000 ) ;
#12614 = CARTESIAN_POINT ( 'NONE',  ( 6.225185179353265319, 13.76374128849115941, -1.297207482702341652 ) ) ;
#12615 = CARTESIAN_POINT ( 'NONE',  ( 2.053005267516999902E-14, 28.63049582772000079, 2.160000000000000142 ) ) ;
#12616 = DIRECTION ( 'NONE',  ( 0.000000000000000000, -1.000000000000000000, 0.000000000000000000 ) ) ;
#12617 = ORIENTED_EDGE ( 'NONE', *, *, #22792, .F. ) ;
#12618 = CARTESIAN_POINT ( 'NONE',  ( -17.17989538244000158, -1.375580078895000113, 9.682594755839000200 ) ) ;
#12619 = CARTESIAN_POINT ( 'NONE',  ( -1.972981379884462871, 26.24919170867575602, 0.8522811625499435717 ) ) ;
#12620 = FACE_BOUND ( 'NONE', #10336, .T. ) ;
#12621 = VERTEX_POINT ( 'NONE', #131 ) ;
#12622 = EDGE_CURVE ( 'NONE', #15489, #13137, #19017, .T. ) ;
#12623 = CARTESIAN_POINT ( 'NONE',  ( -21.63275631497000262, 9.168463912656999781, 5.549645297457000304 ) ) ;
#12624 = CARTESIAN_POINT ( 'NONE',  ( 1.048523528441000163, 25.02545588595999959, -1.870813874093000040 ) ) ;
#12625 = CARTESIAN_POINT ( 'NONE',  ( 14.42874905160420340, -1.189975876054675474, -10.24990194960133216 ) ) ;
#12626 = DIRECTION ( 'NONE',  ( -0.9947502446910230223, 0.000000000000000000, 0.1023325494999024060 ) ) ;
#12627 = CARTESIAN_POINT ( 'NONE',  ( 22.47397007865999896, -6.123241711276000920, 9.448760031808999926 ) ) ;
#12628 = DIRECTION ( 'NONE',  ( 0.000000000000000000, 1.000000000000000000, 0.000000000000000000 ) ) ;
#12629 = DIRECTION ( 'NONE',  ( -1.000000000000000000, 0.000000000000000000, 0.000000000000000000 ) ) ;
#12630 = DIRECTION ( 'NONE',  ( 0.000000000000000000, 1.000000000000000000, 0.000000000000000000 ) ) ;
#12631 = CARTESIAN_POINT ( 'NONE',  ( -9.000000000000000000, 22.00000000000000000, 1.000000000000000000 ) ) ;
#12632 = VERTEX_POINT ( 'NONE', #16966 ) ;
#12633 = CARTESIAN_POINT ( 'NONE',  ( 0.2691697527663042266, 24.02083186604081888, -2.518926031034142810 ) ) ;
#12634 = DIRECTION ( 'NONE',  ( 0.000000000000000000, -1.000000000000000000, -1.745863169774000102E-14 ) ) ;
#12635 = ORIENTED_EDGE ( 'NONE', *, *, #12530, .F. ) ;
#12636 = ADVANCED_FACE ( 'NONE', ( #17202 ), #4012, .T. ) ;
#12637 = CARTESIAN_POINT ( 'NONE',  ( 0.000000000000000000, 28.15000000674550051, 0.000000000000000000 ) ) ;
#12638 = CARTESIAN_POINT ( 'NONE',  ( 16.78754166666665526, -5.593745091089892263, -7.278544301236070879 ) ) ;
#12639 = CARTESIAN_POINT ( 'NONE',  ( 21.94695603379666338, -4.650544061505227589, 8.069014881146078011 ) ) ;
#12640 = CARTESIAN_POINT ( 'NONE',  ( 17.90739874975000134, -0.4687343941967000438, -11.09907540322000052 ) ) ;
#12641 =( BOUNDED_SURFACE ( )  B_SPLINE_SURFACE ( 3, 3, ( 
 ( #1102, #18065, #16349, #14185, #14310, #21702, #8867, #23505, #8617, #21582, #8502, #14533, #16237, #21927, #19767, #3177, #12258 ),
 ( #5112, #7034, #8740, #16103, #5339, #6916, #6668, #12727, #23628, #19643, #10442, #9324, #11023, #3752, #7742, #11141, #18755 ),
 ( #16583, #3989, #7258, #22159, #5570, #16698, #22047, #9088, #5456, #10912, #14993, #18527, #16459, #11384, #7494, #1818, #14761 ),
 ( #14879, #12948, #107, #22504, #3530, #22266, #16815, #14651, #13186, #23850, #20345, #22391, #20467, #5682, #2165, #340, #1936 ) ),
 .UNSPECIFIED., .F., .F., .T. ) 
 B_SPLINE_SURFACE_WITH_KNOTS ( ( 4, 4 ),
 ( 4, 1, 1, 1, 1, 1, 1, 1, 1, 1, 1, 1, 1, 1, 4 ),
 ( 0.000000000000000000, 1.000000000000000000 ),
 ( 0.2369161175745000125, 0.2385325641787000017, 0.2467937715444999958, 0.2545547496928000086, 0.2620001226550999762, 0.2692869410311000133, 0.2765143615464999982, 0.2837371216738999724, 0.2910081725563999910, 0.2983850687121999967, 0.3059382517664999690, 0.3138738688366000118, 0.3225287194381999956, 0.3320773268852000304, 0.3323108935713000034 ),
 .UNSPECIFIED. ) 
 GEOMETRIC_REPRESENTATION_ITEM ( )  RATIONAL_B_SPLINE_SURFACE ( (
 ( 1.093547071729999987, 1.093547071729999987, 1.093547071729999987, 1.093547071729999987, 1.093547071729999987, 1.093547071729999987, 1.093547071729999987, 1.093547071729999987, 1.093547071729999987, 1.093547071729999987, 1.093547071729999987, 1.093547071729999987, 1.093547071729999987, 1.093547071729999987, 1.093547071729999987, 1.093547071729999987, 1.093547071729999987),
 ( 0.9688176427565999838, 0.9688176427565999838, 0.9688176427565999838, 0.9688176427565999838, 0.9688176427565999838, 0.9688176427565999838, 0.9688176427565999838, 0.9688176427565999838, 0.9688176427565999838, 0.9688176427565999838, 0.9688176427565999838, 0.9688176427565999838, 0.9688176427565999838, 0.9688176427565999838, 0.9688176427565999838, 0.9688176427565999838, 0.9688176427565999838),
 ( 0.9688176427565999838, 0.9688176427565999838, 0.9688176427565999838, 0.9688176427565999838, 0.9688176427565999838, 0.9688176427565999838, 0.9688176427565999838, 0.9688176427565999838, 0.9688176427565999838, 0.9688176427565999838, 0.9688176427565999838, 0.9688176427565999838, 0.9688176427565999838, 0.9688176427565999838, 0.9688176427565999838, 0.9688176427565999838, 0.9688176427565999838),
 ( 1.093547071729999987, 1.093547071729999987, 1.093547071729999987, 1.093547071729999987, 1.093547071729999987, 1.093547071729999987, 1.093547071729999987, 1.093547071729999987, 1.093547071729999987, 1.093547071729999987, 1.093547071729999987, 1.093547071729999987, 1.093547071729999987, 1.093547071729999987, 1.093547071729999987, 1.093547071729999987, 1.093547071729999987) ) ) 
 REPRESENTATION_ITEM ( '' )  SURFACE ( )  );
#12642 = ORIENTED_EDGE ( 'NONE', *, *, #4203, .F. ) ;
#12643 = VECTOR ( 'NONE', #9116, 1000.000000000000000 ) ;
#12644 = CARTESIAN_POINT ( 'NONE',  ( -11.12363506584999939, -14.39414658121999935, 3.723758764729999893 ) ) ;
#12645 = CARTESIAN_POINT ( 'NONE',  ( 13.50000000000000178, 5.245049793575820019, -7.438478054735814915 ) ) ;
#12646 = CARTESIAN_POINT ( 'NONE',  ( -1.750000000000000000, 7.000000000000000000, 0.000000000000000000 ) ) ;
#12647 = ORIENTED_EDGE ( 'NONE', *, *, #4688, .T. ) ;
#12648 = EDGE_CURVE ( 'NONE', #3390, #1236, #1820, .T. ) ;
#12649 = FACE_OUTER_BOUND ( 'NONE', #10291, .T. ) ;
#12650 = CARTESIAN_POINT ( 'NONE',  ( 20.67620982502827687, -2.254432935689778983, 10.28453417332591258 ) ) ;
#12651 = CARTESIAN_POINT ( 'NONE',  ( -2.404489386789158356, 26.49040384242090695, 3.230569558791225315 ) ) ;
#12652 = CARTESIAN_POINT ( 'NONE',  ( 16.12378973994088938, -5.293627507836296431, -8.912173777944857989 ) ) ;
#12653 = CARTESIAN_POINT ( 'NONE',  ( -19.35014917163000092, -7.793226253172000462, 6.938245049636000417 ) ) ;
#12654 = CARTESIAN_POINT ( 'NONE',  ( 2.256069968103000090, 29.84916353467000150, -0.6321931223507000208 ) ) ;
#12655 = VECTOR ( 'NONE', #7941, 1000.000000000000000 ) ;
#12657 = CIRCLE ( 'NONE', #11495, 2.399999999999999911 ) ;
#12656 = CARTESIAN_POINT ( 'NONE',  ( -17.01752311569999776, -10.30819550402000040, 0.2320531645540999943 ) ) ;
#12658 = ADVANCED_FACE ( 'NONE', ( #13570 ), #2548, .F. ) ;
#12659 = CARTESIAN_POINT ( 'NONE',  ( 1.973751245779984620, 29.85710109731691020, -0.8775164263322219327 ) ) ;
#12660 = ORIENTED_EDGE ( 'NONE', *, *, #634, .F. ) ;
#12661 = CARTESIAN_POINT ( 'NONE',  ( -24.43506354683022508, -1.794296882945331628, 12.50003182001101365 ) ) ;
#12662 = CARTESIAN_POINT ( 'NONE',  ( 22.48399967376405684, 5.010257334270587393, 9.319128840364694355 ) ) ;
#12663 = CIRCLE ( 'NONE', #8796, 4.625000000000000000 ) ;
#12664 = CARTESIAN_POINT ( 'NONE',  ( -0.9357423685147192582, 23.62724388030657252, -1.910385039341345736 ) ) ;
#12665 = ORIENTED_EDGE ( 'NONE', *, *, #9505, .T. ) ;
#12666 = EDGE_CURVE ( 'NONE', #5222, #17203, #6753, .T. ) ;
#12667 = DIRECTION ( 'NONE',  ( -1.000000000000000000, 0.000000000000000000, 0.000000000000000000 ) ) ;
#12668 = DIRECTION ( 'NONE',  ( 0.000000000000000000, 1.000000000000000000, 0.000000000000000000 ) ) ;
#12669 = EDGE_CURVE ( 'NONE', #18419, #18500, #15093, .T. ) ;
#12670 = CARTESIAN_POINT ( 'NONE',  ( -4.838624173045001697, 12.42376152392000321, -0.01103063371175000071 ) ) ;
#12671 = ORIENTED_EDGE ( 'NONE', *, *, #22955, .F. ) ;
#12672 = DIRECTION ( 'NONE',  ( 1.000000000000000000, 0.000000000000000000, 0.000000000000000000 ) ) ;
#12673 = ORIENTED_EDGE ( 'NONE', *, *, #11200, .T. ) ;
#12674 = AXIS2_PLACEMENT_3D ( 'NONE', #20941, #1440, #8838 ) ;
#12675 = CARTESIAN_POINT ( 'NONE',  ( 6.696152422707000618, 29.50000000000000000, 6.000000000000000000 ) ) ;
#12676 = CARTESIAN_POINT ( 'NONE',  ( -14.48091997122309138, -1.686280348636405968, -12.50000494027439046 ) ) ;
#12677 = ORIENTED_EDGE ( 'NONE', *, *, #1870, .F. ) ;
#12678 = ADVANCED_FACE ( 'NONE', ( #23125 ), #18127, .F. ) ;
#12679 = AXIS2_PLACEMENT_3D ( 'NONE', #8321, #9770, #19215 ) ;
#12680 = CARTESIAN_POINT ( 'NONE',  ( -19.27137435357334283, 5.489963247718526063, 7.417229561569652851 ) ) ;
#12681 = ADVANCED_FACE ( 'NONE', ( #7031 ), #22743, .T. ) ;
#12682 = CARTESIAN_POINT ( 'NONE',  ( -20.95579840402999849, 2.757578367990000334, -10.25841757755000039 ) ) ;
#12683 = CARTESIAN_POINT ( 'NONE',  ( -14.33938192233999942, -0.8520670991562999674, -9.663538843295999214 ) ) ;
#12684 = FACE_OUTER_BOUND ( 'NONE', #13869, .T. ) ;
#12685 = CARTESIAN_POINT ( 'NONE',  ( -24.50000000000000000, -1.873582633960999999, -10.39897383761999983 ) ) ;
#12686 = CARTESIAN_POINT ( 'NONE',  ( 2.172617890951596298, 26.60490896355391754, -0.008667336465691470940 ) ) ;
#12687 = CARTESIAN_POINT ( 'NONE',  ( -7.078629509575005585, 15.37751798353000865, 1.431388464268000815 ) ) ;
#12688 = CARTESIAN_POINT ( 'NONE',  ( 1.756867461946528763, 30.68286621462199193, -1.256417070536908653 ) ) ;
#12689 = EDGE_LOOP ( 'NONE', ( #20117, #17389, #19029, #11732, #3865 ) ) ;
#12690 = CARTESIAN_POINT ( 'NONE',  ( 23.49157400021077180, 3.736182324670829669, 8.508904909832841312 ) ) ;
#12691 = CARTESIAN_POINT ( 'NONE',  ( 2.980299236784382355, 14.12173736862491147, 5.353969783937538196 ) ) ;
#12692 = CARTESIAN_POINT ( 'NONE',  ( 13.81123111472108711, 5.253611299945564639, -7.402707599910051783 ) ) ;
#12693 = AXIS2_PLACEMENT_3D ( 'NONE', #13630, #17273, #19462 ) ;
#12694 = CARTESIAN_POINT ( 'NONE',  ( 5.822189159540518411, 14.45422085624546149, -1.902041274716720354 ) ) ;
#12695 = CARTESIAN_POINT ( 'NONE',  ( 1.347456777940000183, 27.86864211382000178, 1.854615231836999945 ) ) ;
#12696 = DIRECTION ( 'NONE',  ( 1.000000000000000000, 0.000000000000000000, 0.000000000000000000 ) ) ;
#12697 = ORIENTED_EDGE ( 'NONE', *, *, #23312, .F. ) ;
#12698 = CARTESIAN_POINT ( 'NONE',  ( -2.579645516591716259, 11.76412175278740158, -4.075715327416034484 ) ) ;
#12699 = CARTESIAN_POINT ( 'NONE',  ( -10.64810398754049281, 15.44157726471785530, 1.506975047069119222 ) ) ;
#12700 = CARTESIAN_POINT ( 'NONE',  ( 11.84553914498074612, 0.8330063648739851612, -8.962484781899275887 ) ) ;
#12701 = ORIENTED_EDGE ( 'NONE', *, *, #20043, .F. ) ;
#12702 = CARTESIAN_POINT ( 'NONE',  ( 2.434931691670793263, 24.36666666666667425, 0.6543697108981854083 ) ) ;
#12703 = CARTESIAN_POINT ( 'NONE',  ( 2.649999999999999911, 26.50000000000000000, 0.000000000000000000 ) ) ;
#12704 = B_SPLINE_CURVE_WITH_KNOTS ( 'NONE', 3,
 ( #20425, #10872, #14609, #5418, #1428, #21774, #20078, #11102, #16186, #23933, #9048, #5639, #3375, #12908, #3834, #14495, #20190, #1898, #3599, #19956, #8825, #12688, #22120, #10982, #18367, #14724, #20306, #7104, #1658, #3710, #11230, #3492, #9165, #16541, #14381, #12568, #23588, #9288, #5528, #16662, #1553, #6991, #8937, #11581, #181, #19070, #2242, #17021, #297, #7820, #9516, #9637, #6236, #420, #17261, #22346, #15073, #2485, #5765, #20657, #4068, #20778, #17140, #20903, #4307, #15190, #22587, #4185, #20543, #11461, #3954, #18838, #18957, #11698, #5992, #2364, #13150, #13376, #11345, #9400, #9754, #9874, #18717, #536, #659, #7942, #15307, #8064, #6110, #22701, #15435, #7703, #13617, #22822, #13504, #21016, #4427, #18608, #2014, #16772, #7571, #14951, #16894, #2127, #22468, #5879, #13264, #2858, #8553, #19693, #17388, #14110, #17509, #17877, #10367, #11944, #23302, #17631, #13739, #16029, #13989, #784, #21137, #2609, #6718, #10241, #8185, #3109, #23188, #902, #6485, #4551, #6606, #4679, #8429, #14233, #19195, #15797, #15911, #6357, #4917, #1028, #21381, #19329, #4797, #10493, #12182, #15669, #13867, #21505, #2738, #19450, #19571, #2976, #12303, #1279, #10119, #8664, #8304, #23422, #17756, #11818, #12065, #23058, #6839, #21629, #21271, #1160, #9998, #15553, #22940, #6963, #18341, #5048, #21976, #12430, #10725, #23671, #11074, #21860, #19813, #7311, #14355, #14582, #16278, #1399, #1523, #7425, #7190, #14808, #9138, #3227, #10610, #20280, #3684, #14467, #17994, #5159, #16153, #18458, #21746, #5390, #23555, #8791, #12541, #19929, #3347, #10955, #18117, #16393, #12775, #1633, #8912, #5271, #1869, #7080, #12659, #14700, #20048, #3464, #10849, #20166, #3572, #18231, #9022, #23784, #1751, #23903, #16514, #22091, #5501, #12879, #9258, #16634, #43, #16865, #5616, #268, #2455, #16743, #4283, #9371, #7674, #15049, #11434, #22442, #18808, #155, #11199, #7546, #12998, #17113, #13237, #18582, #6080, #9607, #3925, #5852, #14924, #16994, #20629, #628, #20399, #2216, #18933, #22319, #15279, #1986, #4040, #510, #22558, #394, #11671, #9728, #7792, #13473, #11318, #17228, #22671, #15162, #19045, #2340, #20519, #20875, #5736, #7912, #20748, #13124, #11552, #8030, #9846, #22202, #5964, #3805, #18693, #2100, #9490, #13349, #4157, #13960, #15524, #15403, #21108, #10091, #21476, #8277, #22793, #15639, #17352, #23277, #3080, #873, #21236, #13836, #6206, #11790, #17478, #1129, #13591, #21354, #23032, #6449, #4400, #22911, #2575, #14082, #755, #12278, #13711, #6691, #20988, #4519, #12155, #2831, #12036, #4770, #10338, #6329, #4649, #17728, #17853, #11912, #19295, #8527, #2708, #19419, #9966, #19667, #10211, #19544, #17604, #999, #19164, #8399, #8157, #15886, #15767, #23156, #6576, #2951, #4891, #10466, #1248, #3631, #13180, #3523, #14986, #14206, #3983, #5020, #11015, #18639, #23395, #7486, #16576, #20569, #10907, #20458, #11377, #22041, #23966, #5797, #7252, #214, #6814, #5450, #5675, #20337, #5563, #14871, #3869, #23842, #18400, #11261, #18749, #12833, #1810, #7372, #21603, #12404, #20115, #8638, #3745, #13062, #14643, #12940, #18291, #1930, #1691, #9435, #14756, #22152, #20227, #11134, #9198, #18520, #16001, #9317, #7609, #9081, #16692, #16452, #101, #22258, #2045, #16806, #22383, #4461, #11851, #15344, #9785, #11730, #4099, #18985, #11496, #4222, #19104, #19231, #17171, #9906, #13292, #9552, #22733, #22855, #20691, #2644, #5906, #11616, #10040, #2516, #6148, #8219, #13651, #2396, #17424, #7852, #21173, #818, #4338, #22972, #15586, #449, #6389, #2279, #21048, #695, #17052, #15469, #4585, #13772, #11978, #566, #6269 ),
 .UNSPECIFIED., .F., .F.,
 ( 4, 2, 2, 2, 1, 1, 1, 2, 2, 2, 2, 1, 2, 2, 2, 2, 1, 1, 1, 2, 2, 2, 2, 1, 1, 1, 2, 2, 2, 2, 1, 2, 2, 2, 2, 2, 2, 1, 1, 1, 1, 2, 2, 2, 2, 2, 1, 1, 1, 2, 2, 2, 2, 1, 2, 2, 2, 2, 1, 1, 1, 2, 2, 2, 2, 2, 2, 2, 2, 2, 2, 1, 1, 1, 2, 2, 2, 1, 1, 2, 2, 2, 2, 2, 2, 2, 1, 1, 2, 2, 2, 1, 1, 1, 2, 2, 2, 2, 1, 2, 2, 2, 2, 2, 2, 2, 1, 1, 1, 2, 2, 2, 1, 1, 1, 2, 2, 2, 2, 2, 2, 2, 2, 2, 2, 2, 2, 2, 2, 2, 2, 1, 1, 1, 2, 2, 2, 2, 2, 2, 2, 1, 1, 1, 1, 2, 2, 2, 2, 1, 2, 2, 2, 2, 1, 2, 2, 2, 2, 2, 1, 1, 1, 2, 2, 2, 1, 1, 2, 2, 2, 2, 1, 2, 2, 2, 2, 1, 1, 2, 2, 2, 2, 1, 1, 1, 2, 2, 2, 2, 1, 1, 1, 2, 2, 2, 2, 1, 1, 1, 2, 2, 2, 2, 1, 1, 1, 1, 2, 2, 2, 2, 2, 2, 2, 1, 1, 1, 1, 2, 2, 2, 2, 1, 1, 1, 2, 2, 2, 2, 1, 1, 1, 2, 2, 2, 2, 1, 1, 1, 2, 2, 2, 2, 2, 1, 1, 2, 2, 2, 2, 1, 1, 1, 1, 1, 2, 2, 2, 2, 2, 1, 2, 2, 2, 2, 1, 1, 1, 2, 2, 2, 2, 2, 1, 1, 2, 2, 2, 2, 2, 2, 2, 4 ),
 ( 0.000000000000000000, 0.03124999999998551853, 0.04687499999997828126, 0.05468749999997467304, 0.05859374999997287586, 0.06054687499997197381, 0.06152343749997152278, 0.06201171874997130767, 0.06249999999997109257, 0.07031249999996704025, 0.07421874999996501410, 0.07617187499996398714, 0.07714843749996350142, 0.07812499999996300182, 0.08593749999995900501, 0.08984374999995702049, 0.09179687499995603517, 0.09277343749995553557, 0.09326171874995527189, 0.09350585937495514699, 0.09374999999995502209, 0.1015624999999509143, 0.1054687499999488465, 0.1074218749999478195, 0.1083984374999472783, 0.1088867187499470285, 0.1091308593749469175, 0.1093749999999468064, 0.1171874999999435313, 0.1210937499999418798, 0.1230468749999410749, 0.1240234374999406586, 0.1249999999999402284, 0.1562499999999271139, 0.1718749999999205358, 0.1796874999999172606, 0.1835937499999156231, 0.1855468749999147904, 0.1865234374999143740, 0.1870117187499141798, 0.1872558593749140965, 0.1873779296874140410, 0.1874999999999139577, 0.1953124999999100719, 0.1992187499999081290, 0.2011718749999071298, 0.2021484374999066580, 0.2026367187499064082, 0.2028808593749062972, 0.2030029296874062417, 0.2031249999999061862, 0.2109374999999031886, 0.2148437499999016898, 0.2167968749999009404, 0.2177734374999005795, 0.2187499999999002187, 0.2265624999998971656, 0.2304687499998956390, 0.2324218749998948619, 0.2333984374998944733, 0.2338867187498942513, 0.2341308593748941680, 0.2343749999998940847, 0.2421874999998911981, 0.2460937499998897549, 0.2499999999998883116, 0.2656249999998824829, 0.2812499999998765987, 0.2968749999998707700, 0.3046874999998678279, 0.3085937499998663847, 0.3105468749998656630, 0.3115234374998652744, 0.3120117187498651079, 0.3122558593748649969, 0.3124999999998648859, 0.3164062499998635536, 0.3183593749998628319, 0.3193359374998624989, 0.3198242187498623323, 0.3203124999998621658, 0.3242187499998608335, 0.3281249999998595568, 0.3359374999998568923, 0.3398437499998555600, 0.3417968749998548939, 0.3427734374998545608, 0.3432617187498543387, 0.3435058593748542277, 0.3437499999998541167, 0.3515624999998508415, 0.3554687499998492317, 0.3574218749998483990, 0.3583984374998480105, 0.3588867187498478439, 0.3593749999998476774, 0.3671874999998447908, 0.3710937499998433475, 0.3730468749998426814, 0.3740234374998423483, 0.3749999999998419598, 0.3906249999998364641, 0.4062499999998309685, 0.4218749999998254174, 0.4296874999998226419, 0.4335937499998212541, 0.4355468749998205880, 0.4365234374998202549, 0.4370117187498200884, 0.4372558593748200328, 0.4374999999998199773, 0.4453124999998176459, 0.4492187499998164246, 0.4511718749998158695, 0.4521484374998155364, 0.4526367187498153699, 0.4531249999998152034, 0.4570312499998141487, 0.4589843749998135936, 0.4599609374998133715, 0.4609374999998131495, 0.4648437499998120948, 0.4667968749998115952, 0.4677734374998113176, 0.4687499999998110400, 0.4765624999998089861, 0.4804687499998079314, 0.4824218749998074318, 0.4843749999998068767, 0.4921874999998047673, 0.4960937499998037681, 0.4980468749998032130, 0.4990234374998029909, 0.4995117187498028799, 0.4997558593748028244, 0.4999999999998027134, 0.5156249999997973843, 0.5312499999997920552, 0.5468749999997866151, 0.5546874999997840616, 0.5585937499997826183, 0.5605468749997819522, 0.5615234374997816191, 0.5620117187497813971, 0.5622558593747812861, 0.5623779296872812861, 0.5624999999997811750, 0.5664062499997789546, 0.5683593749997778444, 0.5693359374997772893, 0.5698242187497769562, 0.5703124999997766231, 0.5742187499997741806, 0.5761718749997730704, 0.5771484374997725153, 0.5776367187497721822, 0.5781249999997718492, 0.5859374999997716271, 0.5898437499997716271, 0.5917968749997716271, 0.5927734374997716271, 0.5932617187497716271, 0.5935058593747716271, 0.5936279296872716271, 0.5937499999997717381, 0.5976562499997720712, 0.5996093749997722933, 0.6005859374997724043, 0.6010742187497725153, 0.6015624999997726263, 0.6054687499997730704, 0.6074218749997732925, 0.6083984374997734035, 0.6088867187497735145, 0.6093749999997735145, 0.6171874999997747357, 0.6210937499997752909, 0.6230468749997755129, 0.6240234374997756239, 0.6245117187497757349, 0.6249999999997758460, 0.6328124999997768452, 0.6367187499997772893, 0.6386718749997775113, 0.6396484374997776223, 0.6401367187497777334, 0.6403808593747777334, 0.6406249999997777334, 0.6484374999997783995, 0.6523437499997787326, 0.6542968749997789546, 0.6552734374997790656, 0.6557617187497790656, 0.6560058593747790656, 0.6562499999997790656, 0.6640624999997800648, 0.6679687499997806199, 0.6699218749997808420, 0.6708984374997809530, 0.6713867187497810640, 0.6716308593747810640, 0.6718749999997810640, 0.6796874999997818412, 0.6835937499997822853, 0.6855468749997825073, 0.6865234374997825073, 0.6870117187497826183, 0.6872558593747827294, 0.6873779296872828404, 0.6874999999997828404, 0.7031249999997902789, 0.7187499999997977174, 0.7343749999998051559, 0.7421874999998088196, 0.7460937499998107070, 0.7480468749998115952, 0.7490234374998120392, 0.7495117187498122613, 0.7497558593748123723, 0.7498779296873123723, 0.7499999999998123723, 0.7578124999998175904, 0.7617187499998201439, 0.7636718749998213651, 0.7646484374998220312, 0.7651367187498223643, 0.7653808593748225864, 0.7656249999998228084, 0.7734374999998279154, 0.7773437499998303579, 0.7792968749998316902, 0.7802734374998323563, 0.7807617187498326894, 0.7810058593748329114, 0.7812499999998331335, 0.7890624999998387956, 0.7929687499998416822, 0.7949218749998431255, 0.7958984374998437916, 0.7963867187498441247, 0.7966308593748443467, 0.7968749999998445688, 0.8046874999998504530, 0.8085937499998534506, 0.8105468749998550049, 0.8115234374998557820, 0.8120117187498561151, 0.8122558593748563371, 0.8124999999998565592, 0.8437499999998797628, 0.8593749999998914202, 0.8671874999998971933, 0.8710937499999001910, 0.8730468749999016342, 0.8740234374999024114, 0.8745117187499027445, 0.8747558593749029665, 0.8749999999999031886, 0.8828124999999086286, 0.8867187499999114042, 0.8886718749999128475, 0.8896484374999135136, 0.8901367187499138467, 0.8906249999999141798, 0.8984374999999198419, 0.9023437499999227285, 0.9042968749999240607, 0.9052734374999248379, 0.9057617187499251710, 0.9060058593749253930, 0.9062499999999256151, 0.9140624999999314992, 0.9179687499999342748, 0.9199218749999357181, 0.9208984374999364952, 0.9213867187499368283, 0.9216308593749370504, 0.9218749999999372724, 0.9296874999999434896, 0.9335937499999467093, 0.9374999999999499289, 0.9687499999999749090, 0.9843749999999874545, 1.000000000000000000 ),
 .UNSPECIFIED. ) ;
#12705 = VECTOR ( 'NONE', #3414, 1000.000000000000000 ) ;
#12706 = CARTESIAN_POINT ( 'NONE',  ( 17.01281392131000203, -9.720744103539999514, -0.4165551917177999774 ) ) ;
#12707 = CARTESIAN_POINT ( 'NONE',  ( 18.82877641267331370, 5.758514806318896895, 8.698589068941570801 ) ) ;
#12708 = CARTESIAN_POINT ( 'NONE',  ( 2.500000000000000000, 29.43419673618999965, 0.000000000000000000 ) ) ;
#12709 = CARTESIAN_POINT ( 'NONE',  ( -0.1830351089131000142, 30.75454386126000017, -2.142918224942000016 ) ) ;
#12710 = CARTESIAN_POINT ( 'NONE',  ( -12.50725636293000065, 6.705474853889000997, -5.997154546401000097 ) ) ;
#12711 = CARTESIAN_POINT ( 'NONE',  ( 13.50000000000000000, -9.682388338819057694, 0.8738273617125053017 ) ) ;
#12712 = ORIENTED_EDGE ( 'NONE', *, *, #12918, .T. ) ;
#12713 = DIRECTION ( 'NONE',  ( 0.000000000000000000, 1.000000000000000000, 0.000000000000000000 ) ) ;
#12714 = CARTESIAN_POINT ( 'NONE',  ( 21.81229861174000106, -4.409328772385999962, -9.829213302973000665 ) ) ;
#12715 = AXIS2_PLACEMENT_3D ( 'NONE', #14727, #22122, #3378 ) ;
#12716 = DIRECTION ( 'NONE',  ( 0.000000000000000000, -1.000000000000000000, 0.000000000000000000 ) ) ;
#12717 = DIRECTION ( 'NONE',  ( -1.000000000000000000, 0.000000000000000000, 0.000000000000000000 ) ) ;
#12718 = CIRCLE ( 'NONE', #11555, 10.59999999999999964 ) ;
#12719 = CARTESIAN_POINT ( 'NONE',  ( 18.75008227645999881, 0.000000000000000000, 0.000000000000000000 ) ) ;
#12720 = CIRCLE ( 'NONE', #18498, 9.651424765286998664 ) ;
#12721 = FACE_OUTER_BOUND ( 'NONE', #21079, .T. ) ;
#12722 = CARTESIAN_POINT ( 'NONE',  ( -23.98160231569000445, 5.441259261708000672, -9.742227938132998588 ) ) ;
#12723 = VERTEX_POINT ( 'NONE', #16456 ) ;
#12724 = LINE ( 'NONE', #12378, #8044 ) ;
#12725 = ORIENTED_EDGE ( 'NONE', *, *, #23121, .F. ) ;
#12726 = CARTESIAN_POINT ( 'NONE',  ( 1.541590903664999956, 24.04481553841000263, 1.514776262644000004 ) ) ;
#12727 = CARTESIAN_POINT ( 'NONE',  ( 5.849408608611998517, 14.13599281491000248, 1.675474256364998693 ) ) ;
#12728 = FACE_OUTER_BOUND ( 'NONE', #11085, .T. ) ;
#12729 = CARTESIAN_POINT ( 'NONE',  ( 6.189313035766128124, 13.92501040246023791, -0.7765889110677386409 ) ) ;
#12730 = CARTESIAN_POINT ( 'NONE',  ( 2.434931691670788823, 27.63333333333332931, -0.6543697108982009514 ) ) ;
#12731 = AXIS2_PLACEMENT_3D ( 'NONE', #2309, #361, #18774 ) ;
#12732 = ORIENTED_EDGE ( 'NONE', *, *, #12808, .T. ) ;
#12733 = CARTESIAN_POINT ( 'NONE',  ( -16.97676503447000229, -7.308902056012999360, 6.489539471208999544 ) ) ;
#12734 =( GEOMETRIC_REPRESENTATION_CONTEXT ( 3 ) GLOBAL_UNCERTAINTY_ASSIGNED_CONTEXT ( ( #5318 ) ) GLOBAL_UNIT_ASSIGNED_CONTEXT ( ( #6293, #17566, #9692 ) ) REPRESENTATION_CONTEXT ( 'NONE', 'WORKASPACE' ) );
#12735 = CYLINDRICAL_SURFACE ( 'NONE', #12478, 7.000000000000000000 ) ;
#12736 = DIRECTION ( 'NONE',  ( -0.000000000000000000, 0.000000000000000000, 1.000000000000000000 ) ) ;
#12737 = ORIENTED_EDGE ( 'NONE', *, *, #20951, .T. ) ;
#12738 = CARTESIAN_POINT ( 'NONE',  ( -19.47751044566000189, -9.410400067285001668, 6.038396183999999778 ) ) ;
#12739 = CARTESIAN_POINT ( 'NONE',  ( 0.8474240257066999460, 25.43235017058999858, 2.175890254930000101 ) ) ;
#12740 = CARTESIAN_POINT ( 'NONE',  ( 14.75769395697458641, 8.804643041191516417, -5.399440270566639555 ) ) ;
#12741 = CIRCLE ( 'NONE', #8881, 9.274346474608000435 ) ;
#12742 = DIRECTION ( 'NONE',  ( 1.000000000000000000, 0.000000000000000000, 0.000000000000000000 ) ) ;
#12743 = CARTESIAN_POINT ( 'NONE',  ( 21.11529060572999938, -10.17976386977000125, 4.723040569265999800 ) ) ;
#12744 = EDGE_CURVE ( 'NONE', #14191, #9876, #7910, .T. ) ;
#12745 = CARTESIAN_POINT ( 'NONE',  ( 6.696152422707000618, 26.50000000000000000, 6.000000000000000000 ) ) ;
#12746 = CARTESIAN_POINT ( 'NONE',  ( 13.69763181055747658, 8.467209252517251983, -3.113060745664182338 ) ) ;
#12747 = DIRECTION ( 'NONE',  ( 1.000000000000000000, 0.000000000000000000, 0.000000000000000000 ) ) ;
#12748 = DIRECTION ( 'NONE',  ( 0.000000000000000000, 1.000000000000000000, 0.000000000000000000 ) ) ;
#12749 = AXIS2_PLACEMENT_3D ( 'NONE', #3146, #19845, #11766 ) ;
#12750 = ORIENTED_EDGE ( 'NONE', *, *, #16515, .T. ) ;
#12751 = CARTESIAN_POINT ( 'NONE',  ( -14.91309832688787829, -8.601256312377522306, -2.840204793172258491 ) ) ;
#12752 = CARTESIAN_POINT ( 'NONE',  ( -2.164939593608601776, 27.99999999999984368, 3.368873696368140713 ) ) ;
#12753 = B_SPLINE_CURVE_WITH_KNOTS ( 'NONE', 3,
 ( #17562, #11995, #16085, #957 ),
 .UNSPECIFIED., .F., .F.,
 ( 4, 4 ),
 ( 0.000000000000000000, 1.000000000000000000 ),
 .UNSPECIFIED. ) ;
#12754 = CONICAL_SURFACE ( 'NONE', #19321, 9.787173237795000702, 0.7982263333994560339 ) ;
#12755 = ORIENTED_EDGE ( 'NONE', *, *, #14686, .F. ) ;
#12756 = CARTESIAN_POINT ( 'NONE',  ( -15.76749577250665268, 7.930452343988175556, -4.570681609295893288 ) ) ;
#12757 = CARTESIAN_POINT ( 'NONE',  ( 2.299241366213215620, 30.70075862423665569, -0.3023531701502548130 ) ) ;
#12758 = EDGE_CURVE ( 'NONE', #13776, #5466, #10502, .T. ) ;
#12759 = LINE ( 'NONE', #9007, #21634 ) ;
#12760 = CARTESIAN_POINT ( 'NONE',  ( 13.97130829811999853, -6.225248563364000454, -9.070390281432999302 ) ) ;
#12761 = CARTESIAN_POINT ( 'NONE',  ( -15.14443833155225860, 1.225503469059798345, -10.30197729002023443 ) ) ;
#12762 = ORIENTED_EDGE ( 'NONE', *, *, #143, .T. ) ;
#12763 = CARTESIAN_POINT ( 'NONE',  ( -9.079811138770001122, 14.12775011938999903, -4.287383359707000352 ) ) ;
#12764 = DIRECTION ( 'NONE',  ( -0.000000000000000000, 0.8660254037844288266, 0.5000000000000169864 ) ) ;
#12765 = CARTESIAN_POINT ( 'NONE',  ( 0.6838519463944332522, 28.13336607547026702, -4.223839491861407502 ) ) ;
#12766 = AXIS2_PLACEMENT_3D ( 'NONE', #11354, #7828, #10009 ) ;
#12767 = ORIENTED_EDGE ( 'NONE', *, *, #22831, .T. ) ;
#12768 = CARTESIAN_POINT ( 'NONE',  ( 23.64708303493075903, 9.358955864019327109, -4.992123380202468041 ) ) ;
#12769 = DIRECTION ( 'NONE',  ( 1.000000000000000000, 0.000000000000000000, 0.000000000000000000 ) ) ;
#12770 = CARTESIAN_POINT ( 'NONE',  ( 16.10813149828275925, -5.761241547484484471, -8.613496363008477985 ) ) ;
#12771 = CARTESIAN_POINT ( 'NONE',  ( -18.37512077250666565, -9.142823527519007953, 1.196665853474645713 ) ) ;
#12772 = EDGE_CURVE ( 'NONE', #6250, #3348, #15396, .T. ) ;
#12773 = CARTESIAN_POINT ( 'NONE',  ( -2.031444841857999783, 30.28078565870999839, 1.167369564227999978 ) ) ;
#12774 = CARTESIAN_POINT ( 'NONE',  ( -12.71102772709999940, -0.8480750162247000512, -9.618334173012000221 ) ) ;
#12775 = CARTESIAN_POINT ( 'NONE',  ( 1.769171358304295394, 29.88179273471633124, -1.240663272628178770 ) ) ;
#12776 = ORIENTED_EDGE ( 'NONE', *, *, #5842, .F. ) ;
#12777 = CARTESIAN_POINT ( 'NONE',  ( -1.792464842300000027, 23.90299219745999793, 1.497497242616000257 ) ) ;
#12778 = CARTESIAN_POINT ( 'NONE',  ( 20.01551529510171434, 3.913198373954541509, -9.761947581437320665 ) ) ;
#12779 = CARTESIAN_POINT ( 'NONE',  ( -0.8632614635461032249, 23.63695097697195280, -1.954829944972962696 ) ) ;
#12780 = ORIENTED_EDGE ( 'NONE', *, *, #11278, .F. ) ;
#12781 = SHAPE_REPRESENTATION ( 'Stem Lock Nut', ( #4390 ), #9795 ) ;
#12782 = DIRECTION ( 'NONE',  ( 0.000000000000000000, 0.000000000000000000, -1.000000000000000000 ) ) ;
#12783 = CARTESIAN_POINT ( 'NONE',  ( -5.708827511056002280, 14.62924567951000121, 4.675388362802000763 ) ) ;
#12784 = EDGE_CURVE ( 'NONE', #9532, #11090, #16559, .T. ) ;
#12785 = CARTESIAN_POINT ( 'NONE',  ( -1.453122705278999671, 11.52960387473001447, -4.636509077308001103 ) ) ;
#12786 = EDGE_LOOP ( 'NONE', ( #22240, #3200, #21840, #15359, #9439, #22365, #18797, #4563 ) ) ;
#12787 = CARTESIAN_POINT ( 'NONE',  ( 18.30262625730999915, -5.463569446885998993, 7.195226492777999638 ) ) ;
#12788 = ORIENTED_EDGE ( 'NONE', *, *, #13076, .T. ) ;
#12789 = DIRECTION ( 'NONE',  ( 0.000000000000000000, 1.000000000000000000, 0.000000000000000000 ) ) ;
#12790 = EDGE_CURVE ( 'NONE', #13009, #2875, #19876, .T. ) ;
#12791 = PLANE ( 'NONE',  #4397 ) ;
#12792 = ORIENTED_EDGE ( 'NONE', *, *, #5645, .T. ) ;
#12793 = CARTESIAN_POINT ( 'NONE',  ( 22.96733103379666829, 7.405359927155213740, -5.691203335971525945 ) ) ;
#12794 = CARTESIAN_POINT ( 'NONE',  ( -24.75788625869999748, 5.695182633683000262, -8.469459980026998736 ) ) ;
#12795 = EDGE_CURVE ( 'NONE', #15500, #22071, #14647, .T. ) ;
#12796 = CARTESIAN_POINT ( 'NONE',  ( -17.58946748986000230, 9.198462325352998903, -3.355076284083000182 ) ) ;
#12797 = CYLINDRICAL_SURFACE ( 'NONE', #10015, 12.44999999999999929 ) ;
#12798 = EDGE_CURVE ( 'NONE', #7168, #16445, #10776, .T. ) ;
#12799 = CARTESIAN_POINT ( 'NONE',  ( -24.03576324725467117, 10.56622451174204791, -1.538538087633267493 ) ) ;
#12800 = CARTESIAN_POINT ( 'NONE',  ( -1.940745759242866963, 27.86371367745754668, 0.9740794332273453593 ) ) ;
#12801 = CARTESIAN_POINT ( 'NONE',  ( -23.74465998031000069, 13.93375672974000068, -0.8660254037843999608 ) ) ;
#12802 = CARTESIAN_POINT ( 'NONE',  ( -0.8545932710616226391, 29.89685207198636618, 4.125402498422515052 ) ) ;
#12803 = ORIENTED_EDGE ( 'NONE', *, *, #10973, .T. ) ;
#12804 = CARTESIAN_POINT ( 'NONE',  ( -14.25243324638999809, 7.716878364870000340, 11.63397459621999985 ) ) ;
#12805 = CYLINDRICAL_SURFACE ( 'NONE', #16571, 3.000000000000000000 ) ;
#12806 = CARTESIAN_POINT ( 'NONE',  ( 14.65123321485445729, -3.417938325912019515, 8.433851502399324573 ) ) ;
#12807 = CARTESIAN_POINT ( 'NONE',  ( -2.234660536879999881, 26.26021896306000158, 0.4903019467995999303 ) ) ;
#12808 = EDGE_CURVE ( 'NONE', #15539, #13137, #20603, .T. ) ;
#12809 = LINE ( 'NONE', #637, #11560 ) ;
#12810 = CARTESIAN_POINT ( 'NONE',  ( 3.768907243589071143, 12.07611331052141068, 3.028204989709172068 ) ) ;
#12811 = ORIENTED_EDGE ( 'NONE', *, *, #19797, .F. ) ;
#12812 = CARTESIAN_POINT ( 'NONE',  ( 0.9507570701814898051, 11.52082522333564185, -4.719524835566960341 ) ) ;
#12813 = CARTESIAN_POINT ( 'NONE',  ( 4.000000000000000000, 28.30000000000000071, 2.309401076759000304 ) ) ;
#12814 = DIRECTION ( 'NONE',  ( 0.000000000000000000, 1.000000000000000000, 0.000000000000000000 ) ) ;
#12815 = ORIENTED_EDGE ( 'NONE', *, *, #14578, .T. ) ;
#12816 = DIRECTION ( 'NONE',  ( 0.000000000000000000, -1.000000000000000000, 0.000000000000000000 ) ) ;
#12817 = LINE ( 'NONE', #18168, #8858 ) ;
#12818 = CARTESIAN_POINT ( 'NONE',  ( 17.03925158531000150, -7.718145806856000490, 6.728824147386999854 ) ) ;
#12819 = CARTESIAN_POINT ( 'NONE',  ( 18.56467270447140905, 10.41527438795320215, 0.6637449761490703537 ) ) ;
#12820 = EDGE_CURVE ( 'NONE', #7147, #3183, #2248, .T. ) ;
#12821 = CARTESIAN_POINT ( 'NONE',  ( 4.000000142207500886, 28.05137445130360518, 0.9449696197344532589 ) ) ;
#12822 = CARTESIAN_POINT ( 'NONE',  ( -2.309787837468000316, 29.47020436186999959, 0.3857820856266000464 ) ) ;
#12823 = EDGE_CURVE ( 'NONE', #10102, #18875, #12724, .T. ) ;
#12824 = CARTESIAN_POINT ( 'NONE',  ( 24.00016455292000117, 0.000000000000000000, 0.000000000000000000 ) ) ;
#12825 = CARTESIAN_POINT ( 'NONE',  ( 13.49999999999999822, -9.280155195632126208, 3.398040422365634416 ) ) ;
#12826 = ORIENTED_EDGE ( 'NONE', *, *, #2163, .F. ) ;
#12827 = CARTESIAN_POINT ( 'NONE',  ( 0.000000000000000000, 26.35000000000000142, 0.000000000000000000 ) ) ;
#12828 = CARTESIAN_POINT ( 'NONE',  ( 24.01968146971000095, 10.82136356335000116, 3.464147784671999908 ) ) ;
#12829 = LINE ( 'NONE', #20222, #22034 ) ;
#12830 = CARTESIAN_POINT ( 'NONE',  ( 24.50000000000000355, -5.745916189485869019, 8.881438032232539470 ) ) ;
#12831 = CARTESIAN_POINT ( 'NONE',  ( 24.50000000000000000, -2.116736914405999759, 10.36413001332999961 ) ) ;
#12832 = CARTESIAN_POINT ( 'NONE',  ( -4.911757422161000974, 12.43820115989000463, -0.1548696107648001308 ) ) ;
#12833 = CARTESIAN_POINT ( 'NONE',  ( -0.2898344006641048187, 29.22106918680644938, -2.140405143612640337 ) ) ;
#12834 = CARTESIAN_POINT ( 'NONE',  ( 0.000000000000000000, 23.50000000000000000, 0.000000000000000000 ) ) ;
#12835 = EDGE_LOOP ( 'NONE', ( #10522, #20505, #801, #9063 ) ) ;
#12836 = EDGE_CURVE ( 'NONE', #8097, #367, #16566, .T. ) ;
#12837 = DIRECTION ( 'NONE',  ( 0.000000000000000000, -1.000000000000000000, 1.493818482293000218E-14 ) ) ;
#12838 = ORIENTED_EDGE ( 'NONE', *, *, #16152, .T. ) ;
#12839 = CARTESIAN_POINT ( 'NONE',  ( 3.099999999996000177, 22.00000000000000000, 5.570939916054706312E-07 ) ) ;
#12840 = CARTESIAN_POINT ( 'NONE',  ( 11.83261479512859005, -4.444106517313184845, -12.50001436053571346 ) ) ;
#12841 = LINE ( 'NONE', #18411, #8409 ) ;
#12842 = CARTESIAN_POINT ( 'NONE',  ( 15.61599999999999966, 9.072019050554999353, 0.000000000000000000 ) ) ;
#12843 = CARTESIAN_POINT ( 'NONE',  ( 14.95518908531000157, 0.8306535110907999897, 10.15076156001000207 ) ) ;
#12844 = VERTEX_POINT ( 'NONE', #7855 ) ;
#12845 = CARTESIAN_POINT ( 'NONE',  ( -13.92980981492000048, 8.913287911097999228, 3.799313832512000388 ) ) ;
#12846 = CARTESIAN_POINT ( 'NONE',  ( -1.989999999999999991, 9.000000000000000000, -7.500000000000000000 ) ) ;
#12847 = DIRECTION ( 'NONE',  ( 0.000000000000000000, 0.000000000000000000, 1.000000000000000000 ) ) ;
#12848 = ORIENTED_EDGE ( 'NONE', *, *, #13164, .F. ) ;
#12849 = CARTESIAN_POINT ( 'NONE',  ( -21.70527800856000056, 4.716435154626999804, 10.20496424891999965 ) ) ;
#12850 = CARTESIAN_POINT ( 'NONE',  ( -0.8096296179201000198, 24.64120919954999778, 1.985911886929999870 ) ) ;
#12851 = CARTESIAN_POINT ( 'NONE',  ( 14.42389269608120550, -1.357837271329138895, -10.22827832841361584 ) ) ;
#12852 = DIRECTION ( 'NONE',  ( 0.000000000000000000, 0.000000000000000000, -1.000000000000000000 ) ) ;
#12853 = CARTESIAN_POINT ( 'NONE',  ( 24.74930449899000351, -6.846379809230999314, 9.016502796240001061 ) ) ;
#12854 = CARTESIAN_POINT ( 'NONE',  ( 1.474730788452000008, 29.79525031396000045, -1.589135993989999829 ) ) ;
#12855 = CARTESIAN_POINT ( 'NONE',  ( 13.90630400283265189, 8.447665157146255765, 3.286514732384385962 ) ) ;
#12856 = DIRECTION ( 'NONE',  ( 0.000000000000000000, 1.000000000000000000, 0.000000000000000000 ) ) ;
#12857 = CARTESIAN_POINT ( 'NONE',  ( -21.54372087121332058, 7.376325515330552030, -5.668572789218019103 ) ) ;
#12858 = ORIENTED_EDGE ( 'NONE', *, *, #11327, .T. ) ;
#12859 = DIRECTION ( 'NONE',  ( 0.000000000000000000, 0.000000000000000000, -1.000000000000000000 ) ) ;
#12860 = ORIENTED_EDGE ( 'NONE', *, *, #14438, .T. ) ;
#12861 = CARTESIAN_POINT ( 'NONE',  ( -16.52332910583999848, -9.095302903661998783, 0.000000000000000000 ) ) ;
#12862 = CARTESIAN_POINT ( 'NONE',  ( 11.10357421856111770, -11.32461805837665914, -5.385126951711886711 ) ) ;
#12863 = DIRECTION ( 'NONE',  ( 1.000000000000000000, 0.000000000000000000, 0.000000000000000000 ) ) ;
#12864 = CARTESIAN_POINT ( 'NONE',  ( 18.74199463705999946, 10.75162630220000182, 2.884222835622999526 ) ) ;
#12865 = CARTESIAN_POINT ( 'NONE',  ( -14.22336750299141350, -1.721665810523229201, 10.20748740977781743 ) ) ;
#12866 = CARTESIAN_POINT ( 'NONE',  ( -1.812210406530999851, 26.78462896666999882, 1.960438172911999954 ) ) ;
#12867 = VERTEX_POINT ( 'NONE', #7613 ) ;
#12868 = CARTESIAN_POINT ( 'NONE',  ( -9.698120065846001836, -12.55614823169000083, 7.962473021397999062 ) ) ;
#12869 = CARTESIAN_POINT ( 'NONE',  ( -0.2740810853920948031, 6.782218762059497585, -1.732684817544354550 ) ) ;
#12870 = CARTESIAN_POINT ( 'NONE',  ( -14.46758738162252200, -11.92463202973427450, -4.345869468076080544 ) ) ;
#12871 = ORIENTED_EDGE ( 'NONE', *, *, #13758, .F. ) ;
#12872 = CARTESIAN_POINT ( 'NONE',  ( 22.97054755148782235, -10.09263782147366406, -3.219215513880642643 ) ) ;
#12873 = VECTOR ( 'NONE', #4874, 1000.000000000000000 ) ;
#12874 = CARTESIAN_POINT ( 'NONE',  ( 24.36881528991178669, 9.280258940103371046, -8.926120008345273860 ) ) ;
#12875 = CARTESIAN_POINT ( 'NONE',  ( 15.98668428079841419, -8.741113912782290996, -5.559642979276560482 ) ) ;
#12876 = CARTESIAN_POINT ( 'NONE',  ( -14.65290298080999953, 10.85889821503999997, -1.812136570545000103 ) ) ;
#12877 = CARTESIAN_POINT ( 'NONE',  ( -14.25243324638999809, -13.93375672974000068, 0.8660254037843999608 ) ) ;
#12878 = CARTESIAN_POINT ( 'NONE',  ( -17.42378381163999990, -1.451785825221999948, 10.21952336923999916 ) ) ;
#12879 = CARTESIAN_POINT ( 'NONE',  ( 2.161923304883017760, 29.80033983020846478, 0.05993981612989816160 ) ) ;
#12880 = VERTEX_POINT ( 'NONE', #4225 ) ;
#12881 = CARTESIAN_POINT ( 'NONE',  ( -0.1642833103220000257, 23.62380113545999905, -2.215518340065000036 ) ) ;
#12882 = CARTESIAN_POINT ( 'NONE',  ( 22.05839891882162362, 9.896157607257229927, -4.111721767579475717 ) ) ;
#12883 = CARTESIAN_POINT ( 'NONE',  ( -4.000000000000000000, 30.00000000000000000, 0.000000000000000000 ) ) ;
#12884 = VERTEX_POINT ( 'NONE', #15106 ) ;
#12885 = CARTESIAN_POINT ( 'NONE',  ( -0.7409725061051504191, 24.55264775341515104, -2.232429595175999371 ) ) ;
#12886 = CARTESIAN_POINT ( 'NONE',  ( 4.959031697897713364, 14.24213067552161860, -3.859769780926356475 ) ) ;
#12887 = CARTESIAN_POINT ( 'NONE',  ( -4.686714857457999983, 12.36493082504999030, -1.218571946898999281 ) ) ;
#12888 = VERTEX_POINT ( 'NONE', #22156 ) ;
#12889 = EDGE_CURVE ( 'NONE', #16623, #20307, #642, .T. ) ;
#12890 = CARTESIAN_POINT ( 'NONE',  ( 12.37950125730999851, 7.739157895793999487, 4.784640364371000487 ) ) ;
#12891 = ORIENTED_EDGE ( 'NONE', *, *, #18467, .T. ) ;
#12892 = CARTESIAN_POINT ( 'NONE',  ( -4.793505211713778635, 15.72902665353115914, 3.813309186838572451 ) ) ;
#12893 = VECTOR ( 'NONE', #1235, 1000.000000000000000 ) ;
#12894 = APPLICATION_PROTOCOL_DEFINITION ( 'draft international standard', 'automotive_design', 1998, #23802 ) ;
#12895 = CARTESIAN_POINT ( 'NONE',  ( -14.47793696890909310, -1.813149206532627122, -12.49999424749392318 ) ) ;
#12896 = EDGE_LOOP ( 'NONE', ( #20145, #2999, #4228, #3505, #9674, #14877 ) ) ;
#12897 = DIRECTION ( 'NONE',  ( 0.000000000000000000, -1.000000000000000000, 0.000000000000000000 ) ) ;
#12898 = CARTESIAN_POINT ( 'NONE',  ( 12.00000000000000000, -2.131481067915950600, -9.235415327618111903 ) ) ;
#12899 = EDGE_CURVE ( 'NONE', #6008, #15539, #2987, .T. ) ;
#12900 = CARTESIAN_POINT ( 'NONE',  ( -17.79259783783000159, 4.846286003622000571, -8.514261148733998752 ) ) ;
#12901 = DIRECTION ( 'NONE',  ( -1.000000000000000000, 0.000000000000000000, 0.000000000000000000 ) ) ;
#12902 = CARTESIAN_POINT ( 'NONE',  ( -23.23797434907875115, -9.160276637173986103, 5.282797156801545491 ) ) ;
#12903 = CARTESIAN_POINT ( 'NONE',  ( -2.146066666875728668, 27.82396194969284409, 0.3297587073040745276 ) ) ;
#12904 = CARTESIAN_POINT ( 'NONE',  ( 15.88054166666666767, 5.579441265691143848, 7.259931729532359768 ) ) ;
#12906 = AXIS2_PLACEMENT_3D ( 'NONE', #2932, #4380, #13942 ) ;
#12905 = CARTESIAN_POINT ( 'NONE',  ( -6.460109682835006417, 15.34437729315000176, 0.9342512191726000115 ) ) ;
#12907 =( BOUNDED_SURFACE ( )  B_SPLINE_SURFACE ( 3, 3, ( 
 ( #2668, #2794, #588, #8240, #4610, #20710, #4119, #22633, #2305, #4482, #13559, #7873 ),
 ( #11999, #20954, #15607, #8125, #15242, #11517, #19383, #18895, #6174, #2417, #10178, #11637 ),
 ( #15725, #4359, #17565, #717, #5928, #13434, #20836, #9929, #11872, #13313, #11752, #19255 ),
 ( #22875, #9808, #7991, #17192, #22755, #19125, #17444, #2537, #17314, #15490, #838, #6292 ) ),
 .UNSPECIFIED., .F., .F., .T. ) 
 B_SPLINE_SURFACE_WITH_KNOTS ( ( 4, 4 ),
 ( 4, 1, 1, 1, 1, 1, 1, 1, 1, 4 ),
 ( 0.000000000000000000, 1.000000000000000000 ),
 ( 0.2029331708080999996, 0.2146186482909000215, 0.2811902510222000218, 0.3470065005328999974, 0.4101739155435999984, 0.4723427673776999791, 0.5359290704369999991, 0.6036851897885999740, 0.6764911258172999764, 0.7270516473460000295 ),
 .UNSPECIFIED. ) 
 GEOMETRIC_REPRESENTATION_ITEM ( )  RATIONAL_B_SPLINE_SURFACE ( (
 ( 1.179588279202000045, 1.179588279202000045, 1.179588279202000045, 1.179588279202000045, 1.179588279202000045, 1.179588279202000045, 1.179588279202000045, 1.179588279202000045, 1.179588279202000045, 1.179588279202000045, 1.179588279202000045, 1.179588279202000045),
 ( 0.9401372402659999850, 0.9401372402659999850, 0.9401372402659999850, 0.9401372402659999850, 0.9401372402659999850, 0.9401372402659999850, 0.9401372402659999850, 0.9401372402659999850, 0.9401372402659999850, 0.9401372402659999850, 0.9401372402659999850, 0.9401372402659999850),
 ( 0.9401372402659999850, 0.9401372402659999850, 0.9401372402659999850, 0.9401372402659999850, 0.9401372402659999850, 0.9401372402659999850, 0.9401372402659999850, 0.9401372402659999850, 0.9401372402659999850, 0.9401372402659999850, 0.9401372402659999850, 0.9401372402659999850),
 ( 1.179588279202000045, 1.179588279202000045, 1.179588279202000045, 1.179588279202000045, 1.179588279202000045, 1.179588279202000045, 1.179588279202000045, 1.179588279202000045, 1.179588279202000045, 1.179588279202000045, 1.179588279202000045, 1.179588279202000045) ) ) 
 REPRESENTATION_ITEM ( '' )  SURFACE ( )  );
#12908 = CARTESIAN_POINT ( 'NONE',  ( 1.412639476726861298, 30.71297323210350072, -1.633891639758391801 ) ) ;
#12909 = ORIENTED_EDGE ( 'NONE', *, *, #7191, .T. ) ;
#12910 = CARTESIAN_POINT ( 'NONE',  ( -18.18616243917333009, -7.984589140717944566, -4.602174676763225669 ) ) ;
#12911 = FACE_OUTER_BOUND ( 'NONE', #22235, .T. ) ;
#12912 = CARTESIAN_POINT ( 'NONE',  ( 14.40234370370382422, 4.168452611431005650, 8.082017270204577386 ) ) ;
#12913 = CARTESIAN_POINT ( 'NONE',  ( -21.92954041657237596, 10.88116636271459647, 1.967860641670612587 ) ) ;
#12914 = CARTESIAN_POINT ( 'NONE',  ( 0.4903019467994999547, 28.40521896306000116, -2.234660536879999881 ) ) ;
#12915 = AXIS2_PLACEMENT_3D ( 'NONE', #13823, #21223, #17716 ) ;
#12916 = DIRECTION ( 'NONE',  ( 0.000000000000000000, 0.9420570860200443430, 0.3354525997505800605 ) ) ;
#12917 = ORIENTED_EDGE ( 'NONE', *, *, #4184, .F. ) ;
#12918 = EDGE_CURVE ( 'NONE', #7342, #21878, #9556, .T. ) ;
#12919 = CARTESIAN_POINT ( 'NONE',  ( 0.8312882252666201621, 11.51171045331395959, -4.741665037663635118 ) ) ;
#12920 = CARTESIAN_POINT ( 'NONE',  ( -2.100000000000000089, 29.69999999999999929, 0.000000000000000000 ) ) ;
#12921 = CARTESIAN_POINT ( 'NONE',  ( 1.603553703893112470, 28.72969600569719617, 1.618016667675826525 ) ) ;
#12922 = ORIENTED_EDGE ( 'NONE', *, *, #19169, .F. ) ;
#12923 = CYLINDRICAL_SURFACE ( 'NONE', #2603, 1.500000000000001332 ) ;
#12924 = CARTESIAN_POINT ( 'NONE',  ( 15.94237658530999902, 1.989471272253999778, -10.01494924120000007 ) ) ;
#12925 = CARTESIAN_POINT ( 'NONE',  ( 18.02254691115746255, -2.403045170833804978, -10.14401436518803656 ) ) ;
#12926 = ADVANCED_FACE ( 'NONE', ( #22620 ), #23126, .T. ) ;
#12927 = CARTESIAN_POINT ( 'NONE',  ( 4.000000000000000000, 28.30000000000000071, 2.309401076759000304 ) ) ;
#12928 = CARTESIAN_POINT ( 'NONE',  ( 0.4649696821386000156, 28.87458687759999876, 2.295119936837000107 ) ) ;
#12929 = CARTESIAN_POINT ( 'NONE',  ( -12.49041039833999989, 7.040504484191000500, -5.593205555032000120 ) ) ;
#12930 = CARTESIAN_POINT ( 'NONE',  ( 13.50000000000000000, -9.612102684847110723, -0.6144775398871813454 ) ) ;
#12931 = VERTEX_POINT ( 'NONE', #9675 ) ;
#12932 = CARTESIAN_POINT ( 'NONE',  ( 5.155714003469999973, 13.97328511022999997, 4.008150528822999270 ) ) ;
#12933 = CARTESIAN_POINT ( 'NONE',  ( 20.65574852876999756, 3.825724961307999994, 10.60128487009999887 ) ) ;
#12934 = LINE ( 'NONE', #5328, #10828 ) ;
#12935 = ORIENTED_EDGE ( 'NONE', *, *, #10961, .T. ) ;
#12936 = CARTESIAN_POINT ( 'NONE',  ( 0.000000000000000000, 26.34999999328000087, 0.000000000000000000 ) ) ;
#12937 = CARTESIAN_POINT ( 'NONE',  ( 23.01485185659291233, 35.51856778792605240, -6.000000000000000000 ) ) ;
#12938 = VECTOR ( 'NONE', #20896, 1000.000000000000000 ) ;
#12939 = CARTESIAN_POINT ( 'NONE',  ( -1.956099473965003055, 11.60247837895001766, 4.451137785169001937 ) ) ;
#12940 = CARTESIAN_POINT ( 'NONE',  ( 0.2397730383284118749, 29.18954072692674018, -2.146720939784232840 ) ) ;
#12941 = CARTESIAN_POINT ( 'NONE',  ( -19.97157321695999954, 10.67346343640000050, 2.860045257361000015 ) ) ;
#12942 = ORIENTED_EDGE ( 'NONE', *, *, #10313, .F. ) ;
#12943 = CARTESIAN_POINT ( 'NONE',  ( -11.00000000000000000, -7.000000000000000000, 0.000000000000000000 ) ) ;
#12944 = AXIS2_PLACEMENT_3D ( 'NONE', #7763, #127, #5823 ) ;
#12945 = ORIENTED_EDGE ( 'NONE', *, *, #4039, .F. ) ;
#12946 = CARTESIAN_POINT ( 'NONE',  ( -2.109346313336999845, 24.70761240519000168, 1.043221774710999972 ) ) ;
#12947 = ADVANCED_FACE ( 'NONE', ( #16811 ), #302, .T. ) ;
#12948 = CARTESIAN_POINT ( 'NONE',  ( 6.642413157096004106, 13.49915274099000229, -0.03986506147346999263 ) ) ;
#12949 = CARTESIAN_POINT ( 'NONE',  ( 0.000000000000000000, -1.550000000000000044, 0.000000000000000000 ) ) ;
#12950 = EDGE_CURVE ( 'NONE', #7342, #20095, #17055, .T. ) ;
#12951 = CARTESIAN_POINT ( 'NONE',  ( -5.833999999999999631, 1.198997689148999791E-14, 1.310996564781999865E-13 ) ) ;
#12952 = CARTESIAN_POINT ( 'NONE',  ( -14.70932910584000020, -9.048752088456000209, 0.000000000000000000 ) ) ;
#12953 = CARTESIAN_POINT ( 'NONE',  ( 17.61412674930999955, -9.816082492500997958, -4.416083812485999793 ) ) ;
#12954 = ORIENTED_EDGE ( 'NONE', *, *, #6458, .T. ) ;
#12955 = CARTESIAN_POINT ( 'NONE',  ( -15.96111329461999695, 9.155832847151000209, -3.339520933045000195 ) ) ;
#12956 = AXIS2_PLACEMENT_3D ( 'NONE', #3736, #16334, #18741 ) ;
#12957 = DIRECTION ( 'NONE',  ( 0.000000000000000000, -1.000000000000000000, 0.000000000000000000 ) ) ;
#12958 = DIRECTION ( 'NONE',  ( -0.9967542221350019771, 0.000000000000000000, -0.08050478654122018851 ) ) ;
#12959 = VERTEX_POINT ( 'NONE', #12943 ) ;
#12960 = ADVANCED_FACE ( 'NONE', ( #5679, #217 ), #5801, .T. ) ;
#12961 = CARTESIAN_POINT ( 'NONE',  ( -22.39074495098999762, 3.695816561226999752, -10.63704688588000025 ) ) ;
#12962 = EDGE_CURVE ( 'NONE', #1045, #19401, #13848, .T. ) ;
#12963 = CARTESIAN_POINT ( 'NONE',  ( 1.354564830409000109, 24.66385679777999940, 1.902051882269999883 ) ) ;
#12964 = CARTESIAN_POINT ( 'NONE',  ( 14.78385631704689551, 9.271102238192243661, -4.553591355444472022 ) ) ;
#12965 = CARTESIAN_POINT ( 'NONE',  ( 30.87226923053214378, 35.51856778792605240, 0.000000000000000000 ) ) ;
#12966 = CARTESIAN_POINT ( 'NONE',  ( 24.87166914097000259, -9.526620184668999514, 5.135842298655000526 ) ) ;
#12967 = CARTESIAN_POINT ( 'NONE',  ( -2.209175327471999850, 30.73332322239999925, 0.9911013963042000219 ) ) ;
#12968 = CARTESIAN_POINT ( 'NONE',  ( 13.70420460113422401, 8.535173263265548371, -2.924258408944889531 ) ) ;
#12969 = FACE_OUTER_BOUND ( 'NONE', #9152, .T. ) ;
#12970 = CARTESIAN_POINT ( 'NONE',  ( 11.06619116165479255, 11.07450388076360248, -5.818393174638943677 ) ) ;
#12971 = EDGE_LOOP ( 'NONE', ( #16619, #5814, #13273, #4030 ) ) ;
#12972 = CARTESIAN_POINT ( 'NONE',  ( -14.81254764687445302, -7.118814266998854556, -5.616278725454130871 ) ) ;
#12973 = B_SPLINE_CURVE_WITH_KNOTS ( 'NONE', 3,
 ( #800, #8200, #2379, #15085 ),
 .UNSPECIFIED., .F., .F.,
 ( 4, 4 ),
 ( 0.8921488906972279143, 1.000000000000000000 ),
 .UNSPECIFIED. ) ;
#12974 = AXIS2_PLACEMENT_3D ( 'NONE', #4254, #11758, #2543 ) ;
#12975 = CARTESIAN_POINT ( 'NONE',  ( 11.97297107869919941, -13.24884602490436336, 2.052424400535947324 ) ) ;
#12976 = ORIENTED_EDGE ( 'NONE', *, *, #20520, .T. ) ;
#12977 = CARTESIAN_POINT ( 'NONE',  ( 19.75000000000000000, -1.659811535170000019, 9.026773995975998943 ) ) ;
#12978 = DIRECTION ( 'NONE',  ( 0.000000000000000000, 1.000000000000000000, 0.000000000000000000 ) ) ;
#12979 = CARTESIAN_POINT ( 'NONE',  ( 22.06033103379666116, -7.386747355451507069, 5.676899510572770424 ) ) ;
#12980 = CARTESIAN_POINT ( 'NONE',  ( 17.83974014782999973, -10.67906364485000026, -3.053789962008000014 ) ) ;
#12981 = CARTESIAN_POINT ( 'NONE',  ( -23.75388191523000003, -7.467918500480999811, 11.77771164093999978 ) ) ;
#12982 = CARTESIAN_POINT ( 'NONE',  ( -1.733846816785000078, 27.36962896666999967, -2.030073792688000367 ) ) ;
#12983 = ORIENTED_EDGE ( 'NONE', *, *, #16640, .F. ) ;
#12984 = CARTESIAN_POINT ( 'NONE',  ( -9.901765065845999914, -2.260336335250999973, 14.69519359487999921 ) ) ;
#12985 = DIRECTION ( 'NONE',  ( 1.000000000000000000, 0.000000000000000000, 0.000000000000000000 ) ) ;
#12986 = CARTESIAN_POINT ( 'NONE',  ( -14.49454882815139989, -10.37180012737783308, -7.035449704340302368 ) ) ;
#12987 = AXIS2_PLACEMENT_3D ( 'NONE', #10084, #10689, #21714 ) ;
#12988 = ORIENTED_EDGE ( 'NONE', *, *, #12772, .T. ) ;
#12989 = CARTESIAN_POINT ( 'NONE',  ( -24.27585716846455099, 9.160327548063252223, 9.133709619345506070 ) ) ;
#12990 = CARTESIAN_POINT ( 'NONE',  ( 19.26430968566658919, -10.49064719816144198, -0.3961187825285560904 ) ) ;
#12991 = AXIS2_PLACEMENT_3D ( 'NONE', #14588, #14240, #12782 ) ;
#12992 = CARTESIAN_POINT ( 'NONE',  ( 6.243179582884000212, 13.63341776306000064, 1.952383140737000033 ) ) ;
#12993 = CARTESIAN_POINT ( 'NONE',  ( 16.18807664608717545, -3.132089813987705806, -9.878995028433909198 ) ) ;
#12994 = CARTESIAN_POINT ( 'NONE',  ( -18.74007579025000325, 8.211845105499000042, -7.499515029571000468 ) ) ;
#12995 = CARTESIAN_POINT ( 'NONE',  ( 1.319569304714000024, 30.27086167420000251, 1.751203780500999896 ) ) ;
#12996 = CARTESIAN_POINT ( 'NONE',  ( -16.00187137585000130, 9.645521962609000965, 3.562832264799999926 ) ) ;
#12997 = PRODUCT_RELATED_PRODUCT_CATEGORY ( 'part', '', ( #13851 ) ) ;
#12998 = CARTESIAN_POINT ( 'NONE',  ( 1.284731885223538095, 29.68481603961470228, 1.736443197320483911 ) ) ;
#12999 = ORIENTED_EDGE ( 'NONE', *, *, #9180, .F. ) ;
#13000 = CARTESIAN_POINT ( 'NONE',  ( 1.625542394206999974, 24.11238549395999797, 1.677209909501000240 ) ) ;
#13001 = CARTESIAN_POINT ( 'NONE',  ( 21.88815861684361863, 5.936906186455843226, -8.917737836111772509 ) ) ;
#13002 = LINE ( 'NONE', #14704, #9156 ) ;
#13003 = VERTEX_POINT ( 'NONE', #16695 ) ;
#13004 = CARTESIAN_POINT ( 'NONE',  ( -5.458617562394002753, 14.91827681947001771, 3.239474778739999117 ) ) ;
#13005 = CIRCLE ( 'NONE', #10308, 12.89775331292476857 ) ;
#13006 = AXIS2_PLACEMENT_3D ( 'NONE', #415, #2358, #18601 ) ;
#13007 = DIRECTION ( 'NONE',  ( 0.000000000000000000, 0.000000000000000000, -1.000000000000000000 ) ) ;
#13008 = CARTESIAN_POINT ( 'NONE',  ( 18.54843892131000160, -5.767951301206999837, 7.596080989717999721 ) ) ;
#13009 = VERTEX_POINT ( 'NONE', #11138 ) ;
#13010 = CARTESIAN_POINT ( 'NONE',  ( -4.246233029694164607, 15.22475462804525037, 4.414853621744755152 ) ) ;
#13011 = FACE_OUTER_BOUND ( 'NONE', #9567, .T. ) ;
#13012 = VERTEX_POINT ( 'NONE', #7376 ) ;
#13013 = CONICAL_SURFACE ( 'NONE', #2577, 4.309401076758999416, 1.119376321708719590 ) ;
#13014 = CARTESIAN_POINT ( 'NONE',  ( 22.43824770046333938, -7.394682124757493646, -5.682679906726310293 ) ) ;
#13015 = CARTESIAN_POINT ( 'NONE',  ( -0.1118455922670000408, 11.62596257264000421, 4.769745589915999062 ) ) ;
#13016 = AXIS2_PLACEMENT_3D ( 'NONE', #22132, #1670, #193 ) ;
#13017 = CARTESIAN_POINT ( 'NONE',  ( -24.06354693424999880, -6.852501536825999828, 6.820264521660000412 ) ) ;
#13018 = CARTESIAN_POINT ( 'NONE',  ( -19.21451027362000019, 9.383283592320998068, 2.951452985934999607 ) ) ;
#13019 = CARTESIAN_POINT ( 'NONE',  ( 0.000000000000000000, 22.00131761696259503, -2.948682383037075194 ) ) ;
#13020 = DIRECTION ( 'NONE',  ( 0.000000000000000000, 1.000000000000000000, 0.000000000000000000 ) ) ;
#13021 = CYLINDRICAL_SURFACE ( 'NONE', #9669, 2.500000000000000000 ) ;
#13022 = VECTOR ( 'NONE', #1996, 1000.000000000000000 ) ;
#13023 = CARTESIAN_POINT ( 'NONE',  ( 0.000000000000000000, 28.00000000000000000, -4.618802153517000519 ) ) ;
#13024 = EDGE_CURVE ( 'NONE', #2137, #11779, #20055, .T. ) ;
#13025 = CARTESIAN_POINT ( 'NONE',  ( 0.000000000000000000, 21.50000000000000000, 0.000000000000000000 ) ) ;
#13026 = VERTEX_POINT ( 'NONE', #13065 ) ;
#13027 = CARTESIAN_POINT ( 'NONE',  ( -17.46812077250666562, 9.119548119916148110, -1.193619109744021412 ) ) ;
#13028 = FACE_OUTER_BOUND ( 'NONE', #9554, .T. ) ;
#13029 = B_SPLINE_CURVE_WITH_KNOTS ( 'NONE', 3,
 ( #16307, #20192, #12336, #21776, #5300, #3601, #1187, #17789, #5075, #14143, #19840, #19728, #12690, #20081, #16422, #17906, #21662, #6872, #12457, #8939, #8698 ),
 .UNSPECIFIED., .F., .F.,
 ( 4, 2, 2, 2, 2, 2, 2, 2, 2, 1, 4 ),
 ( 0.000000000000000000, 0.1250000000000000833, 0.2500000000000001110, 0.3750000000000001110, 0.5000000000000001110, 0.5625000000000001110, 0.6250000000000002220, 0.7500000000000001110, 0.8125000000000001110, 0.8750000000000000000, 1.000000000000000000 ),
 .UNSPECIFIED. ) ;
#13030 = CARTESIAN_POINT ( 'NONE',  ( 1.670812126161404620, 24.75820121222832526, 1.340034817297290903 ) ) ;
#13031 = CARTESIAN_POINT ( 'NONE',  ( -23.80388666801320596, 10.58805584965292645, -0.3166584334353429453 ) ) ;
#13032 = CARTESIAN_POINT ( 'NONE',  ( 1.902247796447000150, 28.30771896306000102, -1.271041439915000071 ) ) ;
#13033 = CARTESIAN_POINT ( 'NONE',  ( -10.90000000000000036, 1.358133300253999998E-14, 0.000000000000000000 ) ) ;
#13034 = VECTOR ( 'NONE', #14995, 999.9999999999998863 ) ;
#13035 = CARTESIAN_POINT ( 'NONE',  ( 3.749887601161898232, 12.07028453061897544, 3.051358318113421397 ) ) ;
#13036 = ORIENTED_EDGE ( 'NONE', *, *, #15985, .T. ) ;
#13037 = CARTESIAN_POINT ( 'NONE',  ( 0.3785172659374461679, 11.48892188479672072, -4.796579582458316615 ) ) ;
#13038 = ADVANCED_FACE ( 'NONE', ( #20463 ), #10797, .F. ) ;
#13039 = CARTESIAN_POINT ( 'NONE',  ( 0.000000000000000000, 18.72912878474779319, 0.000000000000000000 ) ) ;
#13040 = AXIS2_PLACEMENT_3D ( 'NONE', #15954, #23348, #12353 ) ;
#13041 = CARTESIAN_POINT ( 'NONE',  ( -2.277683716954383986, 29.23235820488807946, 0.03738910628819932386 ) ) ;
#13042 = VERTEX_POINT ( 'NONE', #20572 ) ;
#13043 = DIRECTION ( 'NONE',  ( 0.000000000000000000, 1.000000000000000000, 0.000000000000000000 ) ) ;
#13044 = CARTESIAN_POINT ( 'NONE',  ( 13.41956408531000022, -7.835164430201999153, 6.443409769539999665 ) ) ;
#13045 = CARTESIAN_POINT ( 'NONE',  ( 17.73336492619503701, -9.837232967517808291, -3.444572193406692850 ) ) ;
#13046 = CARTESIAN_POINT ( 'NONE',  ( -2.500000000000000000, 29.03419673619000108, 0.000000000000000000 ) ) ;
#13047 = CARTESIAN_POINT ( 'NONE',  ( -0.8763272250956999354, 30.79866367490999934, -1.893775765471000128 ) ) ;
#13048 = CARTESIAN_POINT ( 'NONE',  ( 0.000000000000000000, 17.95000004008999994, -2.949999959913000236 ) ) ;
#13049 = CARTESIAN_POINT ( 'NONE',  ( -1.713868625172748850, 30.87793769366716035, -1.251725348822291251 ) ) ;
#13050 = CIRCLE ( 'NONE', #8027, 4.750000000000000000 ) ;
#13051 = CIRCLE ( 'NONE', #22333, 1.499999999999999778 ) ;
#13052 = ORIENTED_EDGE ( 'NONE', *, *, #17881, .F. ) ;
#13053 = DIRECTION ( 'NONE',  ( 0.000000000000000000, -1.000000000000000000, 0.000000000000000000 ) ) ;
#13054 = CARTESIAN_POINT ( 'NONE',  ( 20.92705310096999582, 3.648664467165000147, 10.11050619795000038 ) ) ;
#13055 = EDGE_CURVE ( 'NONE', #12531, #6719, #23931, .T. ) ;
#13056 = B_SPLINE_SURFACE_WITH_KNOTS ( 'NONE', 3, 3, ( 
 ( #2978, #17758, #23304, #6841, #6721, #14112, #19695, #21507, #3111, #10495, #1281, #8666, #16032, #14235, #20522, #5855, #4042, #7548, #11202, #22093, #3686, #2219, #14926, #16745, #18343, #9492, #13000, #3807, #157, #12777, #5503, #18584, #16867, #21978, #12881 ),
 ( #15051, #7676, #5618, #270, #13127, #22444, #3574, #22322, #1988, #11076, #5738, #5392, #9140, #16996, #18811, #2102, #3927, #20401, #14810, #20168, #9373, #16517, #396, #11320, #18694, #1753, #13239, #14702, #23905, #20631, #9609, #9260, #14584, #10957, #7313 ),
 ( #20282, #18460, #1872, #16636, #45, #7427, #22204, #21238, #4161, #4651, #7914, #12038, #11554, #19421, #15281, #19047, #2457, #875, #9731, #15165, #6331, #2833, #18935, #6208, #22674, #10093, #10213, #513, #13593, #15526, #2342, #6083, #20990, #20877, #19168 ),
 ( #2578, #2710, #22560, #13475, #8032, #17115, #23034, #17480, #17230, #4285, #11674, #15405, #631, #17606, #9849, #8279, #22795, #7794, #8159, #5966, #9968, #17354, #13839, #758, #22913, #13713, #21110, #4523, #11914, #19297, #15641, #6452, #10341, #17731, #1497 ) ),
 .UNSPECIFIED., .F., .F., .F.,
 ( 4, 4 ),
 ( 4, 1, 1, 1, 1, 1, 1, 1, 1, 1, 1, 1, 1, 1, 1, 1, 1, 1, 1, 1, 1, 1, 1, 1, 1, 1, 1, 1, 1, 1, 1, 1, 4 ),
 ( -0.2678694646895999898, 1.311704223562000005 ),
 ( -0.01431749035882000018, 0.008948431474262000945, 0.03221435330733999486, 0.05548027514042999653, 0.07874619697350999925, 0.1020121188065999940, 0.1252780406396999946, 0.1485439624727999952, 0.1718098843057999925, 0.1950758061388999931, 0.2183417279720000215, 0.2416076498050999943, 0.2648735716381999672, 0.2881394934712000477, 0.3114054153042999928, 0.3346713371373999935, 0.3579372589704999941, 0.3812031808035999947, 0.4044691026366000197, 0.4277350244697000203, 0.4510009463028000209, 0.4742668681359000216, 0.4975327899689999667, 0.5207987118021000228, 0.5440646336350999368, 0.5673305554681999929, 0.5905964773012999380, 0.6138623991343999942, 0.6371283209674999393, 0.6603942428004999643, 0.6836601646335999094, 0.7069260864666999655, 0.7301920082997999106 ),
 .UNSPECIFIED. ) ;
#13057 = DIRECTION ( 'NONE',  ( 0.000000000000000000, 0.000000000000000000, 1.000000000000000000 ) ) ;
#13058 = ORIENTED_EDGE ( 'NONE', *, *, #18997, .F. ) ;
#13059 = CARTESIAN_POINT ( 'NONE',  ( 24.50000000000000000, -3.407821508741362138, 10.10044300661528460 ) ) ;
#13060 = DIRECTION ( 'NONE',  ( 0.000000000000000000, 1.000000000000000000, 0.000000000000000000 ) ) ;
#13061 = CARTESIAN_POINT ( 'NONE',  ( 2.943303094549000853, 11.81758645637001415, 3.952898282072999425 ) ) ;
#13062 = CARTESIAN_POINT ( 'NONE',  ( 0.1497631068246060015, 29.19488348412568968, -2.155278165456777195 ) ) ;
#13063 = CARTESIAN_POINT ( 'NONE',  ( 12.50448585038000004, 13.93375672974000068, -0.4329886192124000055 ) ) ;
#13064 = ORIENTED_EDGE ( 'NONE', *, *, #20646, .F. ) ;
#13065 = CARTESIAN_POINT ( 'NONE',  ( -23.74465998031000069, 7.716878364870000340, 11.63397459621999985 ) ) ;
#13066 = ORIENTED_EDGE ( 'NONE', *, *, #20816, .T. ) ;
#13067 = CARTESIAN_POINT ( 'NONE',  ( -1.592552173163000129, 25.43822112891999510, 1.461104491376000070 ) ) ;
#13068 = FACE_OUTER_BOUND ( 'NONE', #18942, .T. ) ;
#13069 = EDGE_CURVE ( 'NONE', #1109, #11394, #13775, .T. ) ;
#13070 = CARTESIAN_POINT ( 'NONE',  ( 16.08924770046332853, 7.264394122832348977, 5.582553128935895614 ) ) ;
#13071 = CARTESIAN_POINT ( 'NONE',  ( 4.625000000000000000, 15.00000000000000000, 0.000000000000000000 ) ) ;
#13072 = CARTESIAN_POINT ( 'NONE',  ( 0.000000000000000000, 17.89999999999999858, 0.000000000000000000 ) ) ;
#13073 = DIRECTION ( 'NONE',  ( -0.5000000000000169864, 0.000000000000000000, -0.8660254037844289376 ) ) ;
#13074 = CARTESIAN_POINT ( 'NONE',  ( -2.000000000000000000, 30.00000000000000000, -3.464101615137999968 ) ) ;
#13075 = CARTESIAN_POINT ( 'NONE',  ( 4.549999999999999822, 24.49999999999999645, 0.000000000000000000 ) ) ;
#13076 = EDGE_CURVE ( 'NONE', #6250, #7505, #10004, .T. ) ;
#13077 = COLOUR_RGB ( '', 0.31764706, 0.68627451, 0.89019608) ;
#13078 = CARTESIAN_POINT ( 'NONE',  ( -14.25243324638999809, 6.216878364870000340, 12.50000000000000000 ) ) ;
#13079 = ORIENTED_EDGE ( 'NONE', *, *, #10881, .F. ) ;
#13080 = CARTESIAN_POINT ( 'NONE',  ( -22.90484515781000141, -11.18753571154999982, -1.400055669627999988 ) ) ;
#13081 = CARTESIAN_POINT ( 'NONE',  ( -2.076645445633999998, 23.70193952168000351, 0.1838767006059000009 ) ) ;
#13082 = CARTESIAN_POINT ( 'NONE',  ( 4.829987487923999900, 14.79876397742000016, -3.766541047082999860 ) ) ;
#13083 = AXIS2_PLACEMENT_3D ( 'NONE', #2474, #2593, #11686 ) ;
#13084 = CARTESIAN_POINT ( 'NONE',  ( -18.14247087121333735, 1.196138244234068893, -9.136853272523239866 ) ) ;
#13085 = CARTESIAN_POINT ( 'NONE',  ( 19.50029330511999959, -8.080914015124001537, -7.722743123546000454 ) ) ;
#13086 = EDGE_CURVE ( 'NONE', #21017, #4023, #19489, .T. ) ;
#13087 = CARTESIAN_POINT ( 'NONE',  ( -0.7558401036728000788, 30.51789656560000097, -2.438651476941999796 ) ) ;
#13088 = CARTESIAN_POINT ( 'NONE',  ( 14.17388432423843980, 2.487224340016167545, 8.704718658459677627 ) ) ;
#13089 = ADVANCED_FACE ( 'NONE', ( #8105 ), #4464, .F. ) ;
#13090 = DIRECTION ( 'NONE',  ( 0.000000000000000000, -1.000000000000000000, 0.000000000000000000 ) ) ;
#13091 = VECTOR ( 'NONE', #939, 1000.000000000000114 ) ;
#13092 = LINE ( 'NONE', #18664, #19131 ) ;
#13093 = CARTESIAN_POINT ( 'NONE',  ( 11.36701043059670013, 9.445581393796846470, -8.639701956129112403 ) ) ;
#13094 = ORIENTED_EDGE ( 'NONE', *, *, #23928, .T. ) ;
#13095 = CARTESIAN_POINT ( 'NONE',  ( 11.90008533511401012, -13.14613689767216620, 2.230302227742338328 ) ) ;
#13096 = VERTEX_POINT ( 'NONE', #21419 ) ;
#13097 = AXIS2_PLACEMENT_3D ( 'NONE', #20453, #5218, #3741 ) ;
#13098 = DIRECTION ( 'NONE',  ( 0.000000000000000000, 1.000000000000000000, 0.000000000000000000 ) ) ;
#13099 = ADVANCED_FACE ( 'NONE', ( #4834 ), #3073, .F. ) ;
#13100 = CARTESIAN_POINT ( 'NONE',  ( -1.182434930542719087, 29.94682129341587284, -3.936123028068912344 ) ) ;
#13101 = CONICAL_SURFACE ( 'NONE', #17753, 4.309401076758999416, 1.119376321708719590 ) ;
#13102 = VECTOR ( 'NONE', #17160, 1000.000000000000000 ) ;
#13103 = CARTESIAN_POINT ( 'NONE',  ( 13.72319879834999945, -6.784451854297000040, 8.651728039901000145 ) ) ;
#13104 = PLANE ( 'NONE',  #14473 ) ;
#13105 = CARTESIAN_POINT ( 'NONE',  ( 2.554499528901000183, 25.51712896667000052, -0.7744564004552999537 ) ) ;
#13106 = CLOSED_SHELL ( 'NONE', ( #322, #23403, #4008, #23108 ) ) ;
#13107 = VERTEX_POINT ( 'NONE', #23221 ) ;
#13108 = ORIENTED_EDGE ( 'NONE', *, *, #20912, .T. ) ;
#13109 = CARTESIAN_POINT ( 'NONE',  ( -11.31990613876999952, -14.73339388177000231, 3.811521877444000062 ) ) ;
#13110 = VECTOR ( 'NONE', #11880, 1000.000000000000000 ) ;
#13111 = CARTESIAN_POINT ( 'NONE',  ( 16.80728936713000365, -9.102589883624000677, 0.000000000000000000 ) ) ;
#13112 = DIRECTION ( 'NONE',  ( -0.7071067811873956721, 0.7071067811856958096, 7.036629202178957517E-08 ) ) ;
#13113 = VERTEX_POINT ( 'NONE', #698 ) ;
#13114 = CARTESIAN_POINT ( 'NONE',  ( -14.45529025083970964, 9.532921455391518251, 8.488438081448235195 ) ) ;
#13115 = CARTESIAN_POINT ( 'NONE',  ( 19.17606592695706169, -10.11566850997402156, 2.778547194757770455 ) ) ;
#13116 = CARTESIAN_POINT ( 'NONE',  ( -10.35615758860000035, 0.000000000000000000, 7.000000000000000000 ) ) ;
#13117 = CARTESIAN_POINT ( 'NONE',  ( 16.13030374810696443, -5.090882584321414939, -9.031255120879867704 ) ) ;
#13118 = CARTESIAN_POINT ( 'NONE',  ( -13.89620800253999988, -10.81410884553999985, 1.946053687578000124 ) ) ;
#13119 = AXIS2_PLACEMENT_3D ( 'NONE', #19636, #724, #2923 ) ;
#13120 = CARTESIAN_POINT ( 'NONE',  ( -0.8842211952242999828, 29.57975725467000316, 2.001696468556000141 ) ) ;
#13121 = CIRCLE ( 'NONE', #8100, 3.000000000000000000 ) ;
#13122 = AXIS2_PLACEMENT_3D ( 'NONE', #1925, #16336, #13057 ) ;
#13123 = CARTESIAN_POINT ( 'NONE',  ( -12.86025400554999898, 8.992670415662999517, -4.704867779684000162 ) ) ;
#13124 = CARTESIAN_POINT ( 'NONE',  ( 0.07326045961678868956, 29.60812239200971874, 2.159155182468644352 ) ) ;
#13125 = VERTEX_POINT ( 'NONE', #22737 ) ;
#13126 = B_SPLINE_CURVE_WITH_KNOTS ( 'NONE', 3,
 ( #5015, #12400, #8396, #21350, #19661, #10694, #15762, #23522, #19785, #5245, #23271, #12512, #23152, #14078, #3194, #1490, #6685, #19540, #21472, #6573 ),
 .UNSPECIFIED., .F., .F.,
 ( 4, 2, 2, 2, 2, 2, 2, 2, 2, 4 ),
 ( 0.2677099386182879570, 0.3592461962910020179, 0.4507824539637160788, 0.5423187116364300842, 0.6338549693091439785, 0.7253912269818580949, 0.7711593558182151531, 0.8169274846545721003, 0.9084637423272861056, 1.000000000000000000 ),
 .UNSPECIFIED. ) ;
#13127 = CARTESIAN_POINT ( 'NONE',  ( 0.5683451982577000239, 25.66627813763999910, 2.106144784215999710 ) ) ;
#13128 = CARTESIAN_POINT ( 'NONE',  ( 21.49093124556538470, -7.629915688256811102, -7.503604758355795212 ) ) ;
#13129 = CARTESIAN_POINT ( 'NONE',  ( -19.32479587693500989, -9.395654797978956196, -4.657724768059325449 ) ) ;
#13130 = AXIS2_PLACEMENT_3D ( 'NONE', #9145, #18125, #12668 ) ;
#13131 = ORIENTED_EDGE ( 'NONE', *, *, #17878, .T. ) ;
#13132 = FACE_OUTER_BOUND ( 'NONE', #3689, .T. ) ;
#13133 = ADVANCED_FACE ( 'NONE', ( #15588 ), #19288, .T. ) ;
#13134 = CARTESIAN_POINT ( 'NONE',  ( -13.99999999999999645, -10.04553844607464264, 2.270358494041115449 ) ) ;
#13135 = AXIS2_PLACEMENT_3D ( 'NONE', #11838, #18737, #17282 ) ;
#13136 = CARTESIAN_POINT ( 'NONE',  ( 18.21937642130999890, 4.597142045420999246, 8.611084490720001483 ) ) ;
#13137 = VERTEX_POINT ( 'NONE', #9909 ) ;
#13138 = CARTESIAN_POINT ( 'NONE',  ( -14.25546272797000036, 7.467346636043999730, -11.77804180703000014 ) ) ;
#13139 = CARTESIAN_POINT ( 'NONE',  ( -2.500000000000000000, 29.60000000000000142, 0.000000000000000000 ) ) ;
#13140 = ORIENTED_EDGE ( 'NONE', *, *, #15763, .F. ) ;
#13141 = DIRECTION ( 'NONE',  ( -1.000000000000000000, 0.000000000000000000, 0.000000000000000000 ) ) ;
#13142 = CARTESIAN_POINT ( 'NONE',  ( -4.814347747396997335, 12.64342941097000939, -0.06095846195990003991 ) ) ;
#13143 = AXIS2_PLACEMENT_3D ( 'NONE', #14046, #21439, #4852 ) ;
#13144 = CARTESIAN_POINT ( 'NONE',  ( 12.00000000000000000, 4.372713938407501111, -7.949045871140958397 ) ) ;
#13145 = CARTESIAN_POINT ( 'NONE',  ( 18.69687270046333083, -8.912950770672923184, -2.395158628008459800 ) ) ;
#13146 = LINE ( 'NONE', #6106, #16195 ) ;
#13147 = DIRECTION ( 'NONE',  ( 0.000000000000000000, 1.000000000000000000, 0.000000000000000000 ) ) ;
#13148 = CARTESIAN_POINT ( 'NONE',  ( 5.278705197451656339, 13.81926695668341942, -4.223825586974010449 ) ) ;
#13149 = DIRECTION ( 'NONE',  ( 1.000000000000000000, 0.000000000000000000, 0.000000000000000000 ) ) ;
#13150 = CARTESIAN_POINT ( 'NONE',  ( 0.4694942836120984397, 30.43170351587815503, 2.108251680744269940 ) ) ;
#13151 = ORIENTED_EDGE ( 'NONE', *, *, #3639, .T. ) ;
#13152 = CARTESIAN_POINT ( 'NONE',  ( -17.58149577250666695, 7.971127812682293090, -4.594125483385558262 ) ) ;
#13153 = CARTESIAN_POINT ( 'NONE',  ( 24.23273247979999923, -6.599590995379000624, -6.390628695050000196 ) ) ;
#13154 = CARTESIAN_POINT ( 'NONE',  ( 14.58901083706679991, -1.542589092830730646, 8.966384590779057362 ) ) ;
#13155 = PLANE ( 'NONE',  #18863 ) ;
#13156 = CARTESIAN_POINT ( 'NONE',  ( -22.92026629233681234, -10.50598538670077176, 1.170518972298471239 ) ) ;
#13157 = CARTESIAN_POINT ( 'NONE',  ( 1.620993131148000144, 27.08864211382000065, 1.620993131147000055 ) ) ;
#13158 = DIRECTION ( 'NONE',  ( 0.9999999999999941158, 7.061425694895919264E-12, -1.088544838354987623E-07 ) ) ;
#13159 = ORIENTED_EDGE ( 'NONE', *, *, #12784, .T. ) ;
#13160 = CARTESIAN_POINT ( 'NONE',  ( 0.6509447386268639724, 11.50075708578391698, -4.768141952204850043 ) ) ;
#13161 = CARTESIAN_POINT ( 'NONE',  ( 4.000000000000000000, 28.30000000000000071, -2.309401076759000304 ) ) ;
#13162 = LINE ( 'NONE', #15084, #14942 ) ;
#13163 = VERTEX_POINT ( 'NONE', #11733 ) ;
#13164 = EDGE_CURVE ( 'NONE', #17309, #8412, #21229, .T. ) ;
#13165 = FACE_OUTER_BOUND ( 'NONE', #2281, .T. ) ;
#13166 = CARTESIAN_POINT ( 'NONE',  ( 13.63893908531000143, -10.12407100975999974, -0.7263252697377000633 ) ) ;
#13167 = CARTESIAN_POINT ( 'NONE',  ( -19.28553974680000138, -2.542569097918999876, -10.60900310786000134 ) ) ;
#13168 = CARTESIAN_POINT ( 'NONE',  ( 0.000000000000000000, -1.550000000000000044, 0.000000000000000000 ) ) ;
#13169 = CARTESIAN_POINT ( 'NONE',  ( 17.35926537306000128, 1.492411638035999966, 10.76125290731000028 ) ) ;
#13170 = CARTESIAN_POINT ( 'NONE',  ( -1.491631619277377085, 30.87136588096693046, -1.523986932099241853 ) ) ;
#13171 = ORIENTED_EDGE ( 'NONE', *, *, #9544, .F. ) ;
#13172 = CARTESIAN_POINT ( 'NONE',  ( 0.000000000000000000, 28.30000000000000071, -2.100000000000000089 ) ) ;
#13173 = CARTESIAN_POINT ( 'NONE',  ( 22.07214134601000310, 11.17751647723999930, -1.720558685957000122 ) ) ;
#13174 = CARTESIAN_POINT ( 'NONE',  ( -14.09989322724901051, 9.032303263851988007, 3.309274488355915889E-05 ) ) ;
#13175 = VERTEX_POINT ( 'NONE', #2399 ) ;
#13176 = CARTESIAN_POINT ( 'NONE',  ( -2.100000000000000089, 18.10000000000000142, -2.368343299253000103E-10 ) ) ;
#13177 = DIRECTION ( 'NONE',  ( 0.000000000000000000, -1.000000000000000000, -4.004361744935000256E-13 ) ) ;
#13178 = AXIS2_PLACEMENT_3D ( 'NONE', #23737, #18193, #3417 ) ;
#13179 = CARTESIAN_POINT ( 'NONE',  ( 4.447198537830002074, 12.27562294272000720, 1.915162380135998044 ) ) ;
#13180 = CARTESIAN_POINT ( 'NONE',  ( -1.633777111905726498, 29.31308647643173870, -1.412695173303529339 ) ) ;
#13181 = CARTESIAN_POINT ( 'NONE',  ( -23.62697027523000060, 8.705873425905000573, 6.965082319091999707 ) ) ;
#13182 = EDGE_LOOP ( 'NONE', ( #16967, #3335, #20291, #2186 ) ) ;
#13183 = CARTESIAN_POINT ( 'NONE',  ( 0.000000000000000000, 28.15000000674550051, 0.000000000000000000 ) ) ;
#13184 = VERTEX_POINT ( 'NONE', #11853 ) ;
#13185 = CARTESIAN_POINT ( 'NONE',  ( -0.03700557815484000618, 24.74151833367000108, 2.160944269522000027 ) ) ;
#13186 = CARTESIAN_POINT ( 'NONE',  ( 6.269600329294999774, 13.58666533272000088, 2.205063801677000335 ) ) ;
#13187 = CARTESIAN_POINT ( 'NONE',  ( 0.04450989311250999614, 27.09299822780999989, 2.266578917753999889 ) ) ;
#13188 = CARTESIAN_POINT ( 'NONE',  ( 16.73170603379667298, -8.863736118548766640, 2.382193237844414835 ) ) ;
#13189 = DIRECTION ( 'NONE',  ( 0.000000000000000000, 0.000000000000000000, -1.000000000000000000 ) ) ;
#13190 = DIRECTION ( 'NONE',  ( -1.000000000000000000, -2.775557561562888827E-14, 0.000000000000000000 ) ) ;
#13191 = CARTESIAN_POINT ( 'NONE',  ( 14.21381424931000126, -3.754242569768000415, -9.992333729823998922 ) ) ;
#13192 = ADVANCED_FACE ( 'NONE', ( #6391 ), #16580, .T. ) ;
#13193 = CARTESIAN_POINT ( 'NONE',  ( -14.01132597738000030, -2.550904266876999671, 10.45586863968000024 ) ) ;
#13194 = DIRECTION ( 'NONE',  ( 0.000000000000000000, 0.9998172265789604385, 0.01911840568550923769 ) ) ;
#13195 = CARTESIAN_POINT ( 'NONE',  ( -14.45960645816968082, -2.455948252940329812, 12.49996645506771920 ) ) ;
#13196 = VERTEX_POINT ( 'NONE', #17174 ) ;
#13197 = CARTESIAN_POINT ( 'NONE',  ( -22.04801147977000042, 11.23783126569999880, -0.5540781968215000575 ) ) ;
#13198 = CARTESIAN_POINT ( 'NONE',  ( -0.3313809864660999804, 25.26287442561999796, 2.503738740189999756 ) ) ;
#13199 = CARTESIAN_POINT ( 'NONE',  ( 14.20401836875051060, -8.028458463233919318, -6.472791156920650657 ) ) ;
#13200 = DIRECTION ( 'NONE',  ( 0.000000000000000000, -0.4362437346113740011, 0.8998285414523820025 ) ) ;
#13201 = CARTESIAN_POINT ( 'NONE',  ( 24.93285146195000124, -10.16030646464000142, 2.983129374812000023 ) ) ;
#13202 = CARTESIAN_POINT ( 'NONE',  ( 2.251425272252999488, 29.54619791218000202, 0.7094205924024000742 ) ) ;
#13203 = EDGE_CURVE ( 'NONE', #11791, #20267, #316, .T. ) ;
#13204 = CARTESIAN_POINT ( 'NONE',  ( 14.36820406744966760, -3.431467036491389511, 8.367050089429785231 ) ) ;
#13205 = CARTESIAN_POINT ( 'NONE',  ( 16.98472650148946883, 0.04247749959640340772, 10.43385324419452509 ) ) ;
#13206 = CARTESIAN_POINT ( 'NONE',  ( -1.999167105995446780, 26.71753006952333109, 1.536366799937292305 ) ) ;
#13207 = CARTESIAN_POINT ( 'NONE',  ( -6.838539683285000059, 15.31903379280000088, 1.878299112549000061 ) ) ;
#13208 = CARTESIAN_POINT ( 'NONE',  ( 18.97939153144000102, -4.829087144285000299, 10.28159918154000074 ) ) ;
#13209 = ORIENTED_EDGE ( 'NONE', *, *, #7834, .F. ) ;
#13210 = CARTESIAN_POINT ( 'NONE',  ( -2.653270836322014770, 28.03198827073824972, 3.086600612158311385 ) ) ;
#13211 = ADVANCED_FACE ( 'NONE', ( #7975 ), #4589, .T. ) ;
#13212 = ORIENTED_EDGE ( 'NONE', *, *, #21060, .F. ) ;
#13213 = AXIS2_PLACEMENT_3D ( 'NONE', #3098, #10483, #17870 ) ;
#13214 = CARTESIAN_POINT ( 'NONE',  ( -6.000000000000000000, 28.00000000000000000, -6.000000000000000000 ) ) ;
#13215 = CARTESIAN_POINT ( 'NONE',  ( -14.00000000000000000, 9.030549305586312414, 0.000000000000000000 ) ) ;
#13216 = CARTESIAN_POINT ( 'NONE',  ( 14.65928258853999999, 10.53691696905000086, -3.227074023763999655 ) ) ;
#13217 = LINE ( 'NONE', #20611, #10220 ) ;
#13218 = EDGE_CURVE ( 'NONE', #21240, #19135, #21175, .T. ) ;
#13219 = CARTESIAN_POINT ( 'NONE',  ( -0.3933730402102999513, 27.55669433610000141, 2.844001364980000002 ) ) ;
#13220 = ORIENTED_EDGE ( 'NONE', *, *, #5912, .T. ) ;
#13221 = ORIENTED_EDGE ( 'NONE', *, *, #23927, .T. ) ;
#13222 = CARTESIAN_POINT ( 'NONE',  ( -13.99999999999999645, 4.101844789563358518, -8.303384789743008199 ) ) ;
#13223 = VECTOR ( 'NONE', #229, 1000.000000000000114 ) ;
#13224 = CARTESIAN_POINT ( 'NONE',  ( -12.22893471169000001, 15.49542151714999960, -1.510114813732999828 ) ) ;
#13225 = DIRECTION ( 'NONE',  ( 0.7071067811905932254, 0.7071067811824932603, 1.099460927037990408E-07 ) ) ;
#13226 = CARTESIAN_POINT ( 'NONE',  ( 18.13595603379667054, 1.025616415363163503, 9.176462519624685399 ) ) ;
#13227 = VERTEX_POINT ( 'NONE', #8221 ) ;
#13228 = CARTESIAN_POINT ( 'NONE',  ( -7.500000000000000000, 19.50000000000000000, -1.000000000000000000 ) ) ;
#13229 = CARTESIAN_POINT ( 'NONE',  ( 21.03995603379664914, 4.638822124460471485, -8.048677146799199988 ) ) ;
#13230 = FACE_OUTER_BOUND ( 'NONE', #16798, .T. ) ;
#13231 = CARTESIAN_POINT ( 'NONE',  ( 15.49672992670417848, -4.362109857448412065, 9.420198599912847470 ) ) ;
#13232 = CARTESIAN_POINT ( 'NONE',  ( -16.09820950105999771, 4.896146317806000070, 9.904571738106000112 ) ) ;
#13233 = CARTESIAN_POINT ( 'NONE',  ( -0.9845628394066999745, 29.04793232273999948, -1.959238121737999716 ) ) ;
#13234 = EDGE_CURVE ( 'NONE', #16279, #22896, #11087, .T. ) ;
#13235 = CIRCLE ( 'NONE', #4352, 4.750000000000000000 ) ;
#13236 = CARTESIAN_POINT ( 'NONE',  ( -18.52095171394000062, 10.52702611403999988, -4.436598560839000172 ) ) ;
#13237 = CARTESIAN_POINT ( 'NONE',  ( 1.238547465960351257, 29.68149730498098293, 1.769554945797824796 ) ) ;
#13238 = EDGE_LOOP ( 'NONE', ( #9083, #16270, #5146, #6450, #14086 ) ) ;
#13239 = CARTESIAN_POINT ( 'NONE',  ( 1.518228109745999976, 24.13072729665000082, 1.566484663595000049 ) ) ;
#13240 = CARTESIAN_POINT ( 'NONE',  ( -11.04281598264000053, 1.359882291614000008E-14, 0.000000000000000000 ) ) ;
#13241 = CARTESIAN_POINT ( 'NONE',  ( -18.80389074766395652, 6.775504899648727708, -8.189869853558933599 ) ) ;
#13242 = EDGE_LOOP ( 'NONE', ( #10227, #5640, #16949, #2807 ) ) ;
#13243 = CARTESIAN_POINT ( 'NONE',  ( 8.124934037954998800, 1.125145054518999965E-14, 0.000000000000000000 ) ) ;
#13244 = CARTESIAN_POINT ( 'NONE',  ( -4.988174690688001789, 14.11622277100999234, 4.390520985612999638 ) ) ;
#13245 = CARTESIAN_POINT ( 'NONE',  ( -13.99999999999999822, -9.985610030060415809, 2.514921185572130735 ) ) ;
#13246 = ADVANCED_FACE ( 'NONE', ( #2520 ), #21050, .F. ) ;
#13247 = CARTESIAN_POINT ( 'NONE',  ( 18.10968892130999919, 7.460570333748000493, 6.290326521484000288 ) ) ;
#13248 = EDGE_CURVE ( 'NONE', #8533, #11568, #14731, .T. ) ;
#13249 = ORIENTED_EDGE ( 'NONE', *, *, #792, .F. ) ;
#13250 = CIRCLE ( 'NONE', #1288, 4.000000000000000000 ) ;
#13251 = CARTESIAN_POINT ( 'NONE',  ( -6.018858921593000844, 16.12697589426997880, -0.9718497405647000820 ) ) ;
#13252 = CARTESIAN_POINT ( 'NONE',  ( -6.000000000000000000, 28.00000000000000000, -6.000000000000000000 ) ) ;
#13253 = EDGE_LOOP ( 'NONE', ( #3979, #21948, #22542 ) ) ;
#13254 = CARTESIAN_POINT ( 'NONE',  ( 0.000000000000000000, 21.89999999999999858, -3.000000000000013323 ) ) ;
#13255 = CARTESIAN_POINT ( 'NONE',  ( 23.15628936713000030, 9.265517736846000219, 0.000000000000000000 ) ) ;
#13256 = CARTESIAN_POINT ( 'NONE',  ( -0.1133183553920999731, 11.65492397528000978, 4.844731806490002235 ) ) ;
#13257 = CARTESIAN_POINT ( 'NONE',  ( 12.00000000000000000, -0.6870795729671005381, -9.379734039196923945 ) ) ;
#13258 = CARTESIAN_POINT ( 'NONE',  ( 18.88583103379665928, -5.626836121677762925, -7.321603354489151450 ) ) ;
#13260 = EDGE_CURVE ( 'NONE', #14405, #7168, #18524, .T. ) ;
#13259 = CARTESIAN_POINT ( 'NONE',  ( 0.000000000000000000, 15.00000000000000000, -3.100000000000386002 ) ) ;
#13261 = EDGE_CURVE ( 'NONE', #18177, #19500, #20439, .T. ) ;
#13262 = CARTESIAN_POINT ( 'NONE',  ( 0.3056909699690598115, 26.48398052701158178, -2.383980527013956685 ) ) ;
#13263 = CARTESIAN_POINT ( 'NONE',  ( 23.99062354302999722, -6.216878364870000340, 12.50000000000000000 ) ) ;
#13264 = CARTESIAN_POINT ( 'NONE',  ( -1.051908427655785516, 30.33894127233460125, 1.886895527404444328 ) ) ;
#13265 = VERTEX_POINT ( 'NONE', #11237 ) ;
#13266 = CARTESIAN_POINT ( 'NONE',  ( 23.31903954243999877, 10.35114991066999934, -1.095165573133999981 ) ) ;
#13267 = CARTESIAN_POINT ( 'NONE',  ( 3.328927207363430174, 13.17665712429451652, -5.891523500073148512 ) ) ;
#13268 = AXIS2_PLACEMENT_3D ( 'NONE', #14004, #2625, #10017 ) ;
#13269 = DIRECTION ( 'NONE',  ( 1.000000000000000000, 5.653314293126999632E-09, -4.083276203493999756E-09 ) ) ;
#13270 = CARTESIAN_POINT ( 'NONE',  ( -23.34868829266476808, 0.2602095544171842967, 10.57497587573962861 ) ) ;
#13271 = CARTESIAN_POINT ( 'NONE',  ( 1.852511768836999861, 25.52864211381999837, 0.9439018917105000961 ) ) ;
#13272 = DIRECTION ( 'NONE',  ( -1.000000000000000000, 0.000000000000000000, 0.000000000000000000 ) ) ;
#13273 = ORIENTED_EDGE ( 'NONE', *, *, #20978, .F. ) ;
#13274 = CARTESIAN_POINT ( 'NONE',  ( -18.82872164579986674, -0.8013280645230316246, -10.43343868322613943 ) ) ;
#13275 = DIRECTION ( 'NONE',  ( -1.000000000000000000, 0.000000000000000000, 0.000000000000000000 ) ) ;
#13276 = CARTESIAN_POINT ( 'NONE',  ( 1.549555853195504929, 29.73502040408345337, -1.669765763550722815 ) ) ;
#13277 = ORIENTED_EDGE ( 'NONE', *, *, #954, .F. ) ;
#13278 = CARTESIAN_POINT ( 'NONE',  ( -1.771853452025566655, 26.49970565133012101, 1.763679972769350623 ) ) ;
#13279 = CARTESIAN_POINT ( 'NONE',  ( 15.31068924931000019, -3.145391809039999931, 10.23054077443999965 ) ) ;
#13280 = CARTESIAN_POINT ( 'NONE',  ( 61.60588651278290939, 35.51856778792605240, 6.000000000000000000 ) ) ;
#13281 = LINE ( 'NONE', #15090, #18911 ) ;
#13282 = CARTESIAN_POINT ( 'NONE',  ( 15.46296080085999947, -5.609029392994999696, 9.868489697990998621 ) ) ;
#13283 = CARTESIAN_POINT ( 'NONE',  ( -1.617838176641581693, 30.87517387167590499, -1.378981570155497272 ) ) ;
#13284 = DIRECTION ( 'NONE',  ( -1.000000000000000000, 0.000000000000000000, 0.000000000000000000 ) ) ;
#13285 = CARTESIAN_POINT ( 'NONE',  ( 19.21557844680999949, -0.06227916920583000115, 10.25955241042999866 ) ) ;
#13286 = CIRCLE ( 'NONE', #16759, 4.000000000000000000 ) ;
#13287 = CARTESIAN_POINT ( 'NONE',  ( 4.000000000000117240, 24.49999999999976907, -0.3805779584833442475 ) ) ;
#13288 = ORIENTED_EDGE ( 'NONE', *, *, #13333, .F. ) ;
#13289 = DIRECTION ( 'NONE',  ( 1.345655357976046922E-09, -1.000000000000000000, 0.000000000000000000 ) ) ;
#13290 = DIRECTION ( 'NONE',  ( -1.000000000000000000, 0.000000000000000000, 0.000000000000000000 ) ) ;
#13291 = CARTESIAN_POINT ( 'NONE',  ( -3.628081332548001026, 12.07241784922001315, 3.129844478951998799 ) ) ;
#13292 = CARTESIAN_POINT ( 'NONE',  ( 2.160193564748952966, 29.00404398936455763, -0.001994679732726410866 ) ) ;
#13293 = CARTESIAN_POINT ( 'NONE',  ( -23.43942278056000106, -2.880430617476999799, 10.76542036194000040 ) ) ;
#13294 = ORIENTED_EDGE ( 'NONE', *, *, #5542, .F. ) ;
#13295 = CARTESIAN_POINT ( 'NONE',  ( 1.699999998870999951, 12.90000000000000036, 1.053565372968999991 ) ) ;
#13296 = VERTEX_POINT ( 'NONE', #18615 ) ;
#13297 = VECTOR ( 'NONE', #14424, 1000.000000000000000 ) ;
#13298 = CARTESIAN_POINT ( 'NONE',  ( -20.01879387067656424, -9.049182457752882769, 3.224885811638896982 ) ) ;
#13299 = CARTESIAN_POINT ( 'NONE',  ( -1.723852419406000092, 26.80049822781000302, -1.472309056329999866 ) ) ;
#13300 = DIRECTION ( 'NONE',  ( 0.000000000000000000, 1.000000000000000000, 0.000000000000000000 ) ) ;
#13301 = CARTESIAN_POINT ( 'NONE',  ( 0.000000000000000000, 1.224646799146999965E-14, 0.000000000000000000 ) ) ;
#13302 = CARTESIAN_POINT ( 'NONE',  ( 16.29787674931000296, 5.844090361140000134, -8.997790218903000792 ) ) ;
#13303 = CARTESIAN_POINT ( 'NONE',  ( 0.000000000000000000, 0.000000000000000000, 0.000000000000000000 ) ) ;
#13304 = AXIS2_PLACEMENT_3D ( 'NONE', #12048, #6702, #21367 ) ;
#13305 = CARTESIAN_POINT ( 'NONE',  ( -15.63636876114000351, -8.424167882059999002, 6.770715351507000435 ) ) ;
#13306 = CARTESIAN_POINT ( 'NONE',  ( 0.000000000000000000, 26.50000000000000355, 0.000000000000000000 ) ) ;
#13307 = CARTESIAN_POINT ( 'NONE',  ( 23.99062354302999722, 13.93375672974000068, -0.8660254037843999608 ) ) ;
#13308 = VERTEX_POINT ( 'NONE', #20995 ) ;
#13309 = DIRECTION ( 'NONE',  ( 0.000000000000000000, 1.000000000000000000, 0.000000000000000000 ) ) ;
#13310 = CARTESIAN_POINT ( 'NONE',  ( 2.143849369842000030, 24.75054551040999939, -1.335074848179999885 ) ) ;
#13311 = CARTESIAN_POINT ( 'NONE',  ( 13.58082059198365776, -0.8793308655295314358, 10.28020606850954088 ) ) ;
#13312 = CIRCLE ( 'NONE', #20671, 2.000000000000000000 ) ;
#13313 = CARTESIAN_POINT ( 'NONE',  ( -3.167057169673002104, 13.68010474867000603, -5.212571554903001392 ) ) ;
#13314 = CARTESIAN_POINT ( 'NONE',  ( 19.79353649888999911, -8.086732793196000912, -7.728305058073000389 ) ) ;
#13315 = CARTESIAN_POINT ( 'NONE',  ( 2.281976920270999631, 29.61800679778000145, -0.6039657844537000830 ) ) ;
#13316 = CARTESIAN_POINT ( 'NONE',  ( 14.40372725440316870, -4.444427729678738892, 7.873048769373896860 ) ) ;
#13317 = CARTESIAN_POINT ( 'NONE',  ( -14.00000000000000000, 6.995278287856000254, -5.711120943918999160 ) ) ;
#13318 = TOROIDAL_SURFACE ( 'NONE', #13720, 2.500000000000000000, 0.5500000000000000444 ) ;
#13319 = CARTESIAN_POINT ( 'NONE',  ( -4.749999920006001020, 24.30000007999099765, -4.227385599170000255E-08 ) ) ;
#13320 = ADVANCED_FACE ( 'NONE', ( #3718 ), #10989, .T. ) ;
#13321 = CARTESIAN_POINT ( 'NONE',  ( 1.999167105995449445, 29.51753006952333180, -1.536366799937288530 ) ) ;
#13322 = ORIENTED_EDGE ( 'NONE', *, *, #5853, .T. ) ;
#13323 = CARTESIAN_POINT ( 'NONE',  ( 0.4393762720424909118, 29.81534065533141487, -4.365128144578327429 ) ) ;
#13324 = ORIENTED_EDGE ( 'NONE', *, *, #11094, .T. ) ;
#13325 = CARTESIAN_POINT ( 'NONE',  ( 2.257767744500999818, 25.33650334349000133, -1.547397860518000101 ) ) ;
#13326 = CARTESIAN_POINT ( 'NONE',  ( 0.000000000000000000, 24.39999999221199900, 0.000000000000000000 ) ) ;
#13327 = CYLINDRICAL_SURFACE ( 'NONE', #7626, 2.100000000000000089 ) ;
#13328 = VERTEX_POINT ( 'NONE', #4405 ) ;
#13329 = AXIS2_PLACEMENT_3D ( 'NONE', #3543, #7274, #12742 ) ;
#13330 = CARTESIAN_POINT ( 'NONE',  ( 15.20063528206999948, -0.07838933043231000042, 11.03455842080999894 ) ) ;
#13331 = CARTESIAN_POINT ( 'NONE',  ( -6.133957692552824525, 15.94870493351765006, 1.066878949731052684 ) ) ;
#13332 = CARTESIAN_POINT ( 'NONE',  ( 2.219793368323999871, 27.95462896667000052, -1.483218624018999954 ) ) ;
#13333 = EDGE_CURVE ( 'NONE', #15998, #10829, #8071, .T. ) ;
#13334 = ORIENTED_EDGE ( 'NONE', *, *, #12608, .F. ) ;
#13335 = ORIENTED_EDGE ( 'NONE', *, *, #11768, .F. ) ;
#13336 = CARTESIAN_POINT ( 'NONE',  ( -13.99999999999999645, 3.801362129166840909, -8.462681129871283403 ) ) ;
#13337 = CARTESIAN_POINT ( 'NONE',  ( -12.02528971169000016, 11.32897754936000112, 10.67910005269999907 ) ) ;
#13338 = DIRECTION ( 'NONE',  ( 0.000000000000000000, 0.000000000000000000, 1.000000000000000000 ) ) ;
#13339 = PLANE ( 'NONE',  #17148 ) ;
#13340 = VERTEX_POINT ( 'NONE', #16781 ) ;
#13341 = CARTESIAN_POINT ( 'NONE',  ( -14.38789236265103177, 12.88903867674593684, 2.675117728956161400 ) ) ;
#13342 = CARTESIAN_POINT ( 'NONE',  ( 6.165272352932655409, 14.04219028581453443, 0.4745907567973399188 ) ) ;
#13343 = CARTESIAN_POINT ( 'NONE',  ( 15.63618592470433022, -8.281329406721820163, 6.227711793688024855 ) ) ;
#13344 = CARTESIAN_POINT ( 'NONE',  ( -14.83356629584000075, 7.743367107227999924, -7.832546484073001025 ) ) ;
#13345 = CARTESIAN_POINT ( 'NONE',  ( -2.341484834389000014, 30.80774310834999952, -0.2625247487647999756 ) ) ;
#13346 = AXIS2_PLACEMENT_3D ( 'NONE', #811, #323, #7728 ) ;
#13347 = CARTESIAN_POINT ( 'NONE',  ( -14.78308928803000022, -1.400056168502999965, -10.15245659134999912 ) ) ;
#13348 = EDGE_CURVE ( 'NONE', #20885, #17972, #7304, .T. ) ;
#13349 = CARTESIAN_POINT ( 'NONE',  ( -0.3788180770592776692, 29.58146988764027085, 2.126762119974988430 ) ) ;
#13350 = ORIENTED_EDGE ( 'NONE', *, *, #4764, .T. ) ;
#13351 = CARTESIAN_POINT ( 'NONE',  ( -18.45662066148324953, 9.913592205210392194, 3.361782804926630064 ) ) ;
#13352 = ORIENTED_EDGE ( 'NONE', *, *, #18437, .T. ) ;
#13353 = CARTESIAN_POINT ( 'NONE',  ( -5.483104808914001538, 16.58388603771001613, 3.024255283996999832 ) ) ;
#13354 = FACE_OUTER_BOUND ( 'NONE', #17712, .T. ) ;
#13355 = AXIS2_PLACEMENT_3D ( 'NONE', #9840, #22664, #13585 ) ;
#13356 = EDGE_CURVE ( 'NONE', #18186, #23810, #12809, .T. ) ;
#13357 = CARTESIAN_POINT ( 'NONE',  ( 17.34187642131000118, -3.686089773936000125, -9.013740861256998471 ) ) ;
#13358 = ORIENTED_EDGE ( 'NONE', *, *, #18141, .T. ) ;
#13359 = CONICAL_SURFACE ( 'NONE', #3715, 13.23032192316000000, 1.093540295016705466 ) ;
#13360 = LINE ( 'NONE', #8043, #20666 ) ;
#13361 = FACE_OUTER_BOUND ( 'NONE', #254, .T. ) ;
#13362 = VERTEX_POINT ( 'NONE', #20198 ) ;
#13363 = CARTESIAN_POINT ( 'NONE',  ( -12.50000000000000000, 6.668552375895999695, -6.032891668653000750 ) ) ;
#13364 = B_SPLINE_CURVE_WITH_KNOTS ( 'NONE', 3,
 ( #2594, #4669, #17497, #9986, #15297, #8293, #22688, #15541, #22929, #6346, #2967, #12421, #12053, #6707, #23177, #1388, #3219, #14225, #8545, #6595, #6956, #10357, #23545, #6832, #21370, #12172, #13979, #14099, #21738, #21494, #10601, #4787, #5151, #19562, #1268, #1150, #8418, #17746, #19438, #8655, #2848, #8781 ),
 .UNSPECIFIED., .F., .F.,
 ( 4, 2, 1, 2, 2, 2, 1, 2, 2, 2, 2, 2, 2, 2, 2, 1, 2, 2, 2, 1, 2, 2, 4 ),
 ( 0.000000000000000000, 0.06250000000000038858, 0.09375000000000058287, 0.1093750000000009159, 0.1250000000000012490, 0.1875000000000026090, 0.2187500000000032752, 0.2343750000000035805, 0.2500000000000038303, 0.3125000000000036082, 0.3750000000000033862, 0.5000000000000028866, 0.5625000000000024425, 0.6250000000000021094, 0.6875000000000016653, 0.7187500000000014433, 0.7343750000000013323, 0.7500000000000012212, 0.8125000000000003331, 0.8437500000000000000, 0.8593749999999998890, 0.8749999999999997780, 1.000000000000000000 ),
 .UNSPECIFIED. ) ;
#13365 = CARTESIAN_POINT ( 'NONE',  ( 21.54929166666666163, -1.207328351017986412, 9.224279008625865472 ) ) ;
#13366 = CARTESIAN_POINT ( 'NONE',  ( 4.570970069156997440, 12.55112336938002038, 1.530869126733999108 ) ) ;
#13367 = CARTESIAN_POINT ( 'NONE',  ( -13.99999999999999822, -2.102368047938235840, 9.650932645709392688 ) ) ;
#13368 = EDGE_CURVE ( 'NONE', #20052, #19119, #11647, .T. ) ;
#13369 = CARTESIAN_POINT ( 'NONE',  ( 12.00000000000000000, -4.187907907339877944, -8.648131877027614323 ) ) ;
#13370 = CARTESIAN_POINT ( 'NONE',  ( 19.15037270046332196, 2.398204772357335646, -8.924285576194829872 ) ) ;
#13371 = CARTESIAN_POINT ( 'NONE',  ( -6.215630469039999717, 16.31160401236000368, -1.000000000001000089 ) ) ;
#13372 = CARTESIAN_POINT ( 'NONE',  ( 5.607894170315999460, 13.81677657626999967, 3.376581585463999780 ) ) ;
#13373 = CARTESIAN_POINT ( 'NONE',  ( 5.290861247900399356, 13.79131577112301876, -4.285521124256567838 ) ) ;
#13374 = DIRECTION ( 'NONE',  ( 0.000000000000000000, 0.9995485718789889340, 0.03004417505396965102 ) ) ;
#13375 = EDGE_CURVE ( 'NONE', #18008, #3010, #17750, .T. ) ;
#13376 = CARTESIAN_POINT ( 'NONE',  ( 0.4444477064986781523, 30.43018009420528003, 2.113756326305517685 ) ) ;
#13377 = EDGE_LOOP ( 'NONE', ( #13212, #4384, #1634 ) ) ;
#13378 = EDGE_CURVE ( 'NONE', #9702, #3316, #17976, .T. ) ;
#13379 = CARTESIAN_POINT ( 'NONE',  ( 21.33396847639999905, 9.703104815872000799, 1.500914832134000010 ) ) ;
#13380 = CARTESIAN_POINT ( 'NONE',  ( -1.476145454422083558, 12.87712156297896371, -6.520379654891271137 ) ) ;
#13381 = AXIS2_PLACEMENT_3D ( 'NONE', #18700, #9498, #22452 ) ;
#13382 = CARTESIAN_POINT ( 'NONE',  ( 1.306994031390691813, 29.96241504948190126, 3.864208797664316020 ) ) ;
#13383 = AXIS2_PLACEMENT_3D ( 'NONE', #17627, #17752, #15548 ) ;
#13384 = CARTESIAN_POINT ( 'NONE',  ( -23.58967566784923164, 8.020275622323017828, 6.913969526970511481 ) ) ;
#13385 = CARTESIAN_POINT ( 'NONE',  ( -2.149413090608000232, 28.48696440326000001, 1.203722632180999952 ) ) ;
#13386 = CARTESIAN_POINT ( 'NONE',  ( -2.000000000000000000, 28.00000000000000000, 3.464101615137999968 ) ) ;
#13387 = ORIENTED_EDGE ( 'NONE', *, *, #11058, .T. ) ;
#13388 = CARTESIAN_POINT ( 'NONE',  ( -18.80081040857043462, 0.2165797905031099924, -10.46343287096509833 ) ) ;
#13389 = EDGE_CURVE ( 'NONE', #20864, #18414, #15776, .T. ) ;
#13390 = CARTESIAN_POINT ( 'NONE',  ( 24.50000000000000000, 10.82531754731000007, 6.250000000000000000 ) ) ;
#13391 = AXIS2_PLACEMENT_3D ( 'NONE', #11205, #21980, #7429 ) ;
#13392 = EDGE_CURVE ( 'NONE', #13265, #8938, #9031, .T. ) ;
#13393 = CARTESIAN_POINT ( 'NONE',  ( 1.981941605402921525, 27.97637690296692980, 0.8825957265570513188 ) ) ;
#13394 = DIRECTION ( 'NONE',  ( 0.000000000000000000, -1.000000000000000000, 0.000000000000000000 ) ) ;
#13395 = ORIENTED_EDGE ( 'NONE', *, *, #19013, .F. ) ;
#13396 = DIRECTION ( 'NONE',  ( 5.702240835238999409E-10, 0.9999999999999997780, -2.283934685009999534E-08 ) ) ;
#13397 = AXIS2_PLACEMENT_3D ( 'NONE', #402, #4166, #7434 ) ;
#13398 = CARTESIAN_POINT ( 'NONE',  ( 13.88475174931000033, -10.63832449705000016, -0.7632376485559000390 ) ) ;
#13399 = CARTESIAN_POINT ( 'NONE',  ( -13.93810026219000164, -11.26370332044000122, -0.8539229629768000374 ) ) ;
#13400 = CARTESIAN_POINT ( 'NONE',  ( -10.04281598263999875, 16.40330333352000025, 0.9999999999983999466 ) ) ;
#13401 = CARTESIAN_POINT ( 'NONE',  ( 15.12489037305999950, 10.79910518316000001, -0.2491780114572999805 ) ) ;
#13402 = CARTESIAN_POINT ( 'NONE',  ( 0.000000000000000000, 21.94999982584599962, 0.000000000000000000 ) ) ;
#13403 = DIRECTION ( 'NONE',  ( 1.000000000000000000, 0.000000000000000000, 0.000000000000000000 ) ) ;
#13404 = CARTESIAN_POINT ( 'NONE',  ( 24.56229061411000458, 9.827592947978999405, 3.145925499939000503 ) ) ;
#13405 = CARTESIAN_POINT ( 'NONE',  ( 2.321186682587942141, 30.00000000000000000, 3.278664397485417048 ) ) ;
#13406 = VERTEX_POINT ( 'NONE', #14449 ) ;
#13407 = CIRCLE ( 'NONE', #4439, 0.5500000000000001554 ) ;
#13408 = LINE ( 'NONE', #4335, #1886 ) ;
#13409 = CARTESIAN_POINT ( 'NONE',  ( 2.437990915149000237, 25.92706776952000070, 0.5485649090615000167 ) ) ;
#13410 = CARTESIAN_POINT ( 'NONE',  ( -4.833442993138002741, 12.42174073273999646, -0.1521763619671000767 ) ) ;
#13411 = AXIS2_PLACEMENT_3D ( 'NONE', #14998, #5808, #13190 ) ;
#13412 = CARTESIAN_POINT ( 'NONE',  ( 24.29519417982890772, -9.695549469153794675, -1.137487036544780006 ) ) ;
#13413 = CARTESIAN_POINT ( 'NONE',  ( -21.78904027164999846, 8.063099807893998161, 7.627676736206999486 ) ) ;
#13414 = VERTEX_POINT ( 'NONE', #20263 ) ;
#13415 = AXIS2_PLACEMENT_3D ( 'NONE', #12157, #19904, #21838 ) ;
#13416 = DIRECTION ( 'NONE',  ( -1.000000000000000000, 0.000000000000000000, 0.000000000000000000 ) ) ;
#13417 = ORIENTED_EDGE ( 'NONE', *, *, #8194, .F. ) ;
#13418 = CARTESIAN_POINT ( 'NONE',  ( -23.97728971656852082, 5.151501960897337362, -12.49974207332436116 ) ) ;
#13419 = DIRECTION ( 'NONE',  ( 0.7071067811864980568, -0.7071067811865969777, -1.093189995836995798E-08 ) ) ;
#13420 = CARTESIAN_POINT ( 'NONE',  ( -2.214344957515000267, 26.11799822780999847, 0.4858445502740000310 ) ) ;
#13421 = ADVANCED_FACE ( 'NONE', ( #20148 ), #1848, .T. ) ;
#13422 = CARTESIAN_POINT ( 'NONE',  ( -2.932110437813000292, 12.98378357228998681, 6.429187290204003702 ) ) ;
#13423 = CARTESIAN_POINT ( 'NONE',  ( -1.689767423161654181, 6.985088818113795561, 0.4612040785389939224 ) ) ;
#13424 = CARTESIAN_POINT ( 'NONE',  ( 15.31068924931000019, -3.145391809039999931, 10.23054077443999965 ) ) ;
#13425 = CARTESIAN_POINT ( 'NONE',  ( -12.86025400554999898, 8.992670415662999517, -4.704867779684000162 ) ) ;
#13426 = CARTESIAN_POINT ( 'NONE',  ( 14.02481375730999957, 9.137735611494999688, -0.2793723515763000265 ) ) ;
#13427 = CARTESIAN_POINT ( 'NONE',  ( 24.35625626386761056, 12.44383109334005866, -3.446652305529492200 ) ) ;
#13428 = ORIENTED_EDGE ( 'NONE', *, *, #4688, .F. ) ;
#13429 = CARTESIAN_POINT ( 'NONE',  ( -0.2318060435179999934, 31.07084775298000068, -2.713913184503999876 ) ) ;
#13430 = CIRCLE ( 'NONE', #12679, 7.000000000000000000 ) ;
#13431 = CARTESIAN_POINT ( 'NONE',  ( -0.6445284140762999048, 24.00469973582999827, -2.638471611800000005 ) ) ;
#13432 = CARTESIAN_POINT ( 'NONE',  ( 13.59953730933185589, -1.556863950183797751, 10.19646127995974361 ) ) ;
#13433 = VERTEX_POINT ( 'NONE', #22075 ) ;
#13434 = CARTESIAN_POINT ( 'NONE',  ( 1.774480129771998538, 13.34308553469999659, -5.838396592341002389 ) ) ;
#13435 = CARTESIAN_POINT ( 'NONE',  ( -24.50000000000000000, 14.43375672974000068, 0.000000000000000000 ) ) ;
#13436 = CARTESIAN_POINT ( 'NONE',  ( -1.055980501909000058, 29.22533662481999883, 2.324492492552999945 ) ) ;
#13437 = CARTESIAN_POINT ( 'NONE',  ( 11.12576011242912699, 1.246535810083129636, 12.50000754954551141 ) ) ;
#13438 = CARTESIAN_POINT ( 'NONE',  ( -2.729128784747790970, 18.00000000000000000, 0.000000000000000000 ) ) ;
#13439 = CYLINDRICAL_SURFACE ( 'NONE', #23415, 2.500000000000000000 ) ;
#13440 = CARTESIAN_POINT ( 'NONE',  ( 0.000000000000000000, 21.89999999999999858, 0.000000000000000000 ) ) ;
#13441 = CARTESIAN_POINT ( 'NONE',  ( 24.37173283531061330, -12.35285683711744653, -3.604224339486718609 ) ) ;
#13442 = ORIENTED_EDGE ( 'NONE', *, *, #19155, .F. ) ;
#13443 = CARTESIAN_POINT ( 'NONE',  ( 0.9358744650684699407, 29.91068681084918879, -4.078474779182606369 ) ) ;
#13444 = AXIS2_PLACEMENT_3D ( 'NONE', #6498, #10253, #2751 ) ;
#13445 = ORIENTED_EDGE ( 'NONE', *, *, #22210, .T. ) ;
#13446 = PRODUCT_DEFINITION_SHAPE ( 'NONE', 'NONE',  #23970 ) ;
#13447 = CARTESIAN_POINT ( 'NONE',  ( -5.833999999999999631, 1.198997689148999791E-14, 1.310996564781999865E-13 ) ) ;
#13449 = LINE ( 'NONE', #13689, #15136 ) ;
#13448 = CARTESIAN_POINT ( 'NONE',  ( 0.000000000000000000, 21.87500000000000000, 0.000000000000000000 ) ) ;
#13450 = CARTESIAN_POINT ( 'NONE',  ( 24.06553262398158921, -9.296743367502696032, 1.372136975361484268 ) ) ;
#13451 = CARTESIAN_POINT ( 'NONE',  ( 1.699999998837999904, 12.90000000000000036, -1.053565373074999867 ) ) ;
#13452 = CARTESIAN_POINT ( 'NONE',  ( -7.500000000000000000, 19.50000000000000000, -6.000000000000000000 ) ) ;
#13453 = AXIS2_PLACEMENT_3D ( 'NONE', #4612, #13798, #14050 ) ;
#13454 = CARTESIAN_POINT ( 'NONE',  ( -2.866097959738999723, 26.58169433609999999, 0.1690226414555000001 ) ) ;
#13455 = ORIENTED_EDGE ( 'NONE', *, *, #23433, .F. ) ;
#13456 = ORIENTED_EDGE ( 'NONE', *, *, #18250, .T. ) ;
#13457 = CARTESIAN_POINT ( 'NONE',  ( -14.00000000000000355, 0.5659072664207758230, -9.465469235123730840 ) ) ;
#13458 = FACE_OUTER_BOUND ( 'NONE', #18515, .T. ) ;
#13459 = CARTESIAN_POINT ( 'NONE',  ( -23.74465998031000069, -7.716878364870000340, -11.63397459621999985 ) ) ;
#13460 = EDGE_CURVE ( 'NONE', #14183, #10512, #16962, .T. ) ;
#13461 = EDGE_LOOP ( 'NONE', ( #9401, #5567, #17005, #29 ) ) ;
#13462 = CARTESIAN_POINT ( 'NONE',  ( -18.63160066766000256, -9.081568620942999104, 1.581064911138999829 ) ) ;
#13463 = CARTESIAN_POINT ( 'NONE',  ( -14.43045961913871622, 12.44097983993677659, 3.451577511309273039 ) ) ;
#13464 = FACE_OUTER_BOUND ( 'NONE', #14152, .T. ) ;
#13465 = CARTESIAN_POINT ( 'NONE',  ( 15.75487062095969470, -10.05329925375477806, 2.473809878897430092 ) ) ;
#13466 = AXIS2_PLACEMENT_3D ( 'NONE', #4258, #7648, #11291 ) ;
#13467 = CARTESIAN_POINT ( 'NONE',  ( -15.66879943471000125, -9.824257856382001108, -5.029609084265999286 ) ) ;
#13468 = CARTESIAN_POINT ( 'NONE',  ( 2.052109269678999759, 30.34279869486999814, 0.7725448515828999829 ) ) ;
#13469 = CARTESIAN_POINT ( 'NONE',  ( 30.87226923053214378, 37.01856778792605240, 2.673746900119611247 ) ) ;
#13470 = CARTESIAN_POINT ( 'NONE',  ( -17.30216962611999776, -8.848728181206000798, -7.171245711509000920 ) ) ;
#13471 = AXIS2_PLACEMENT_3D ( 'NONE', #9051, #7107, #18259 ) ;
#13472 = EDGE_CURVE ( 'NONE', #22434, #17213, #10752, .T. ) ;
#13473 = CARTESIAN_POINT ( 'NONE',  ( 0.4691844297121841589, 29.63158630830557172, 2.108311878348199997 ) ) ;
#13474 = ORIENTED_EDGE ( 'NONE', *, *, #3775, .F. ) ;
#13475 = CARTESIAN_POINT ( 'NONE',  ( 1.704131630875000081, 25.52532134332999902, 1.616576773546999801 ) ) ;
#13476 = AXIS2_PLACEMENT_3D ( 'NONE', #8457, #15580, #21410 ) ;
#13477 = CARTESIAN_POINT ( 'NONE',  ( 0.000000000000000000, 18.72912878474779319, 0.000000000000000000 ) ) ;
#13478 = VECTOR ( 'NONE', #11930, 1000.000000000000000 ) ;
#13479 = ORIENTED_EDGE ( 'NONE', *, *, #987, .F. ) ;
#13480 = CARTESIAN_POINT ( 'NONE',  ( -3.317497142792999121, 13.45106591520001160, 5.148782710378998040 ) ) ;
#13481 = AXIS2_PLACEMENT_3D ( 'NONE', #822, #22976, #15348 ) ;
#13482 = CARTESIAN_POINT ( 'NONE',  ( 15.03843892131000004, -8.433581200277000534, 4.746982932527000543 ) ) ;
#13483 = ORIENTED_EDGE ( 'NONE', *, *, #15743, .T. ) ;
#13484 = DIRECTION ( 'NONE',  ( 0.000000000000000000, -1.000000000000000000, 0.000000000000000000 ) ) ;
#13485 = CARTESIAN_POINT ( 'NONE',  ( -9.000000000000000000, 22.00000000000000000, -1.000000000000000000 ) ) ;
#13486 = AXIS2_PLACEMENT_3D ( 'NONE', #14856, #21907, #14744 ) ;
#13487 = EDGE_CURVE ( 'NONE', #4084, #5502, #23540, .T. ) ;
#13488 = ORIENTED_EDGE ( 'NONE', *, *, #14968, .F. ) ;
#13489 = CARTESIAN_POINT ( 'NONE',  ( 4.000000000000000000, 26.47444252552741872, -0.7494995952805646455 ) ) ;
#13490 = CARTESIAN_POINT ( 'NONE',  ( 21.77604166666666075, -7.380913445605565393, 5.672416130782132804 ) ) ;
#13491 = CARTESIAN_POINT ( 'NONE',  ( -4.447536355888999537, 12.50584014757999185, 1.859842023822999568 ) ) ;
#13492 = CARTESIAN_POINT ( 'NONE',  ( -12.49618567022092641, 6.982953552602237046, -5.700977629478201969 ) ) ;
#13494 = CARTESIAN_POINT ( 'NONE',  ( 17.86344468463383350, -7.381542623598233099, -7.407332015522091417 ) ) ;
#13493 = VECTOR ( 'NONE', #11096, 1000.000000000000000 ) ;
#13495 = CARTESIAN_POINT ( 'NONE',  ( 23.99062354302999722, 6.216878364870000340, -12.50000000000000000 ) ) ;
#13496 = CARTESIAN_POINT ( 'NONE',  ( -21.35476253787999923, 9.219287007783998789, 0.000000000000000000 ) ) ;
#13497 = CARTESIAN_POINT ( 'NONE',  ( -4.820916185790466102, 13.26632684913112037, 5.688929395781997300 ) ) ;
#13498 = B_SPLINE_CURVE_WITH_KNOTS ( 'NONE', 3,
 ( #23110, #12359, #10540, #5093, #10657, #18045, #1450, #23234, #13918, #21314, #1081, #8846, #6648, #23609, #17811, #13789, #14043, #21436 ),
 .UNSPECIFIED., .F., .F.,
 ( 4, 2, 2, 2, 2, 2, 2, 2, 4 ),
 ( 0.000000000000000000, 0.1250000000000000555, 0.2500000000000001110, 0.3750000000000000555, 0.5000000000000000000, 0.6249999999999998890, 0.7499999999999998890, 0.8749999999999998890, 1.000000000000000000 ),
 .UNSPECIFIED. ) ;
#13499 = CARTESIAN_POINT ( 'NONE',  ( -14.00000000000000000, 1.396097351027999937E-14, 0.000000000000000000 ) ) ;
#13500 = CIRCLE ( 'NONE', #16981, 2.000000000000000000 ) ;
#13501 = FILL_AREA_STYLE ('',( #22343 ) ) ;
#13502 = CARTESIAN_POINT ( 'NONE',  ( 1.699999998870999951, 12.90000000000000036, 1.053565372968999991 ) ) ;
#13503 = ADVANCED_FACE ( 'NONE', ( #14340, #8896 ), #23534, .T. ) ;
#13504 = CARTESIAN_POINT ( 'NONE',  ( -0.5044265879204176128, 30.37393115978347424, 2.100552943717841181 ) ) ;
#13505 = ORIENTED_EDGE ( 'NONE', *, *, #14246, .F. ) ;
#13506 = CARTESIAN_POINT ( 'NONE',  ( 22.94668360559225562, 9.017902059207619558, 2.425039471787421075 ) ) ;
#13507 = CARTESIAN_POINT ( 'NONE',  ( 3.536817740288733525, 13.22384477141398129, -5.784969809341429681 ) ) ;
#13508 = SPHERICAL_SURFACE ( 'NONE', #5341, 12.50000000000000000 ) ;
#13509 = TOROIDAL_SURFACE ( 'NONE', #10440, 2.500000000000000000, 0.5500000000000000444 ) ;
#13510 = CARTESIAN_POINT ( 'NONE',  ( -1.672139866504000150, 26.92696440325999774, 1.808910716397999829 ) ) ;
#13511 = CIRCLE ( 'NONE', #21260, 4.625000000000000000 ) ;
#13512 = DIRECTION ( 'NONE',  ( 1.000000000000000000, 0.000000000000000000, 0.000000000000000000 ) ) ;
#13513 = ORIENTED_EDGE ( 'NONE', *, *, #8054, .T. ) ;
#13514 = EDGE_CURVE ( 'NONE', #12420, #14786, #1119, .T. ) ;
#13515 = CARTESIAN_POINT ( 'NONE',  ( -17.40524854711295433, -10.32373598890054467, -1.469896786939441924 ) ) ;
#13516 = CARTESIAN_POINT ( 'NONE',  ( 0.000000000000000000, 22.00000000000000000, 0.000000000000000000 ) ) ;
#13517 = CARTESIAN_POINT ( 'NONE',  ( 2.000000000000000000, 24.50000000000000000, 3.464101615137999968 ) ) ;
#13518 = ORIENTED_EDGE ( 'NONE', *, *, #21552, .F. ) ;
#13519 = EDGE_CURVE ( 'NONE', #23889, #1360, #6524, .T. ) ;
#13520 = ORIENTED_EDGE ( 'NONE', *, *, #20509, .T. ) ;
#13521 = EDGE_CURVE ( 'NONE', #21343, #2374, #3555, .T. ) ;
#13522 = CARTESIAN_POINT ( 'NONE',  ( 17.67649770046333657, 9.124895482576970807, -1.194572973190361820 ) ) ;
#13523 = CARTESIAN_POINT ( 'NONE',  ( 16.18818924931000325, 2.089945795291999975, -10.52064088945999920 ) ) ;
#13524 = CARTESIAN_POINT ( 'NONE',  ( -19.48867009477000067, -8.807317413567998798, -6.448376625637000537 ) ) ;
#13525 = CARTESIAN_POINT ( 'NONE',  ( 23.81455253808871930, -9.280040243854974946, -1.185412662895561242 ) ) ;
#13526 = CARTESIAN_POINT ( 'NONE',  ( 13.09364037305999950, 7.670935586994999333, -7.523170208358000544 ) ) ;
#13527 = CARTESIAN_POINT ( 'NONE',  ( 13.50000000000000178, -7.987118333487818411, -4.877847799884814428 ) ) ;
#13528 = CARTESIAN_POINT ( 'NONE',  ( 1.999167105995457216, 26.95086340285667248, 1.536366799937278760 ) ) ;
#13529 = CARTESIAN_POINT ( 'NONE',  ( 21.90655408178999863, -8.810107392619000777, -5.231571157656000004 ) ) ;
#13530 = EDGE_CURVE ( 'NONE', #8805, #16101, #12350, .T. ) ;
#13531 = CARTESIAN_POINT ( 'NONE',  ( 3.999878274658703159, 24.63336607547242707, -1.519686587934146127 ) ) ;
#13532 = ORIENTED_EDGE ( 'NONE', *, *, #9911, .T. ) ;
#13533 = CARTESIAN_POINT ( 'NONE',  ( 12.40372306987999984, 5.542563168401000162, -7.077615733026999756 ) ) ;
#13534 = CARTESIAN_POINT ( 'NONE',  ( -0.2616786785208999877, 26.96706776951999984, -2.656868203660999850 ) ) ;
#13535 = CIRCLE ( 'NONE', #13922, 0.9999999999999992228 ) ;
#13536 = CARTESIAN_POINT ( 'NONE',  ( -4.723119614623001894, 12.53615931869001621, -0.05929000460447006460 ) ) ;
#13537 = LINE ( 'NONE', #15219, #5369 ) ;
#13538 = CARTESIAN_POINT ( 'NONE',  ( -23.29280118367000085, -2.879402575693999822, 10.76157691598000099 ) ) ;
#13539 = ORIENTED_EDGE ( 'NONE', *, *, #20646, .T. ) ;
#13540 = DIRECTION ( 'NONE',  ( 0.000000000000000000, 1.000000000000000000, 0.000000000000000000 ) ) ;
#13541 = ORIENTED_EDGE ( 'NONE', *, *, #22654, .T. ) ;
#13542 = CARTESIAN_POINT ( 'NONE',  ( 0.6284882100611323130, 11.57509495284122458, 4.749874987833288209 ) ) ;
#13543 = CARTESIAN_POINT ( 'NONE',  ( -1.472309056329999866, 27.58049822781000060, -1.723852419406000092 ) ) ;
#13544 = FACE_OUTER_BOUND ( 'NONE', #21901, .T. ) ;
#13545 = CARTESIAN_POINT ( 'NONE',  ( -0.4126679282215456324, 30.83232909844395309, -2.137904739592160652 ) ) ;
#13546 = CARTESIAN_POINT ( 'NONE',  ( 12.89756424930999934, 10.41448860350999972, -2.177620798092000598 ) ) ;
#13547 = EDGE_CURVE ( 'NONE', #9495, #9372, #23149, .T. ) ;
#13548 = EDGE_CURVE ( 'NONE', #21343, #19197, #2262, .T. ) ;
#13549 = CARTESIAN_POINT ( 'NONE',  ( -12.75178580833000019, 5.886008164689000566, -8.319303600761999817 ) ) ;
#13550 = CARTESIAN_POINT ( 'NONE',  ( 13.25700125730999979, -8.207589172378998654, -3.980341215395999832 ) ) ;
#13551 = CARTESIAN_POINT ( 'NONE',  ( -14.49999964368427818, 0.5192523986245470846, 12.50000205182227297 ) ) ;
#13552 = ORIENTED_EDGE ( 'NONE', *, *, #20092, .T. ) ;
#13553 = CARTESIAN_POINT ( 'NONE',  ( 2.696211895155999905, 30.07815194586000018, -0.3869592438285999747 ) ) ;
#13554 = CARTESIAN_POINT ( 'NONE',  ( -1.290484346291000062, 24.83723422303999939, -2.389895288096000048 ) ) ;
#13555 = CARTESIAN_POINT ( 'NONE',  ( 13.85371245318831157, -8.834497878575451324, 5.305004613496619115 ) ) ;
#13556 = AXIS2_PLACEMENT_3D ( 'NONE', #20104, #3733, #1452 ) ;
#13557 = ORIENTED_EDGE ( 'NONE', *, *, #12542, .F. ) ;
#13558 = B_SPLINE_CURVE_WITH_KNOTS ( 'NONE', 3,
 ( #11226, #16768, #13372, #2360, #22696, #22584 ),
 .UNSPECIFIED., .F., .F.,
 ( 4, 1, 1, 4 ),
 ( 0.000000000000000000, 0.3333333333333000081, 0.6666666666667000474, 1.000000000000000000 ),
 .UNSPECIFIED. ) ;
#13559 = CARTESIAN_POINT ( 'NONE',  ( -4.480219250449000157, 13.39360627083002164, -5.444853299477003361 ) ) ;
#13560 = PRESENTATION_STYLE_ASSIGNMENT (( #4120 ) ) ;
#13561 = CARTESIAN_POINT ( 'NONE',  ( 0.3765435872583000054, 29.19171087983999868, 2.719724165663000015 ) ) ;
#13562 = EDGE_CURVE ( 'NONE', #11958, #1386, #12759, .T. ) ;
#13563 = CARTESIAN_POINT ( 'NONE',  ( 11.72559253309398386, 4.116598456381781901, 12.49995860919340274 ) ) ;
#13564 = ADVANCED_FACE ( 'NONE', ( #23882 ), #14648, .T. ) ;
#13565 = CARTESIAN_POINT ( 'NONE',  ( 17.57014765749539720, -9.538208588764241824, -4.608418869076832181 ) ) ;
#13566 = DIRECTION ( 'NONE',  ( 1.000000000000000000, 0.000000000000000000, 0.000000000000000000 ) ) ;
#13567 = CARTESIAN_POINT ( 'NONE',  ( -21.09612077250664086, 9.212649750328886000, -1.205806084666599665 ) ) ;
#13568 = CARTESIAN_POINT ( 'NONE',  ( 23.99999963380712131, 13.93375672974000246, -0.09624782609426597857 ) ) ;
#13569 = ORIENTED_EDGE ( 'NONE', *, *, #9643, .T. ) ;
#13570 = FACE_OUTER_BOUND ( 'NONE', #6607, .T. ) ;
#13571 = ORIENTED_EDGE ( 'NONE', *, *, #13997, .T. ) ;
#13572 = DIRECTION ( 'NONE',  ( 0.000000000000000000, -1.000000000000000000, 0.000000000000000000 ) ) ;
#13573 = CARTESIAN_POINT ( 'NONE',  ( -2.102266727616999731, 23.66000000000000014, 0.4960590750638999569 ) ) ;
#13574 = DIRECTION ( 'NONE',  ( 0.000000000000000000, 0.000000000000000000, -1.000000000000000000 ) ) ;
#13575 = CARTESIAN_POINT ( 'NONE',  ( 15.13297668014999964, 10.44537513801999928, 3.552586481088999992 ) ) ;
#13576 = CARTESIAN_POINT ( 'NONE',  ( -5.847212767158005420, 15.04942523385998498, -2.909050744206997496 ) ) ;
#13577 = CARTESIAN_POINT ( 'NONE',  ( 23.41677564524290744, 35.51856778792605240, 6.000000000000000000 ) ) ;
#13578 = EDGE_LOOP ( 'NONE', ( #8597, #13335, #23109, #10743, #10620, #10450 ) ) ;
#13579 = EDGE_LOOP ( 'NONE', ( #11036, #14367, #2532, #2161, #22043, #12518, #4553, #17967 ) ) ;
#13580 = CARTESIAN_POINT ( 'NONE',  ( -14.00000000000000000, 6.995278287856000254, -5.711120943918999160 ) ) ;
#13581 = CARTESIAN_POINT ( 'NONE',  ( 2.944270284434496787, 29.92936170367566717, -2.918926912232259419 ) ) ;
#13582 = DIRECTION ( 'NONE',  ( 1.000000000000000000, 0.000000000000000000, 0.000000000000000000 ) ) ;
#13583 = VERTEX_POINT ( 'NONE', #15257 ) ;
#13584 = CARTESIAN_POINT ( 'NONE',  ( 1.702253152602459796, 12.92476687935645074, -1.054244267527355117 ) ) ;
#13585 = DIRECTION ( 'NONE',  ( -0.1989999999999970126, 0.9799994897957861051, 0.000000000000000000 ) ) ;
#13586 = CARTESIAN_POINT ( 'NONE',  ( 15.75898575427667581, -10.08917934536900418, 2.323824035917134712 ) ) ;
#13587 = CARTESIAN_POINT ( 'NONE',  ( -17.44139086687999907, -4.785270692951000271, -9.999417235773998769 ) ) ;
#13588 = CARTESIAN_POINT ( 'NONE',  ( -0.9118897615661000211, 29.87256183959000211, -2.172606093380000214 ) ) ;
#13589 = CARTESIAN_POINT ( 'NONE',  ( -20.20122951085723884, 8.831040645199459860, 5.673307061337953705 ) ) ;
#13590 = CARTESIAN_POINT ( 'NONE',  ( -13.97056789615000127, 4.578996057282999743, 9.143398144881999201 ) ) ;
#13591 = CARTESIAN_POINT ( 'NONE',  ( -1.391465838797818266, 29.51483024477171213, 1.652436496091826745 ) ) ;
#13592 = ORIENTED_EDGE ( 'NONE', *, *, #20459, .F. ) ;
#13593 = CARTESIAN_POINT ( 'NONE',  ( -0.7013385995965000230, 23.74705491642000155, 2.070322660781999780 ) ) ;
#13594 = CARTESIAN_POINT ( 'NONE',  ( -19.09328248614785650, -3.188221648232169692, -9.986957848427829632 ) ) ;
#13595 = ORIENTED_EDGE ( 'NONE', *, *, #12918, .F. ) ;
#13596 = CARTESIAN_POINT ( 'NONE',  ( 5.193778049067001135, 13.91699130313997657, -4.147951301185004880 ) ) ;
#13597 = DIRECTION ( 'NONE',  ( -1.000000000000000000, 0.000000000000000000, 0.000000000000000000 ) ) ;
#13598 = CARTESIAN_POINT ( 'NONE',  ( -19.80530420454666540, 5.641336654966718100, -7.340471888469334516 ) ) ;
#13599 = CARTESIAN_POINT ( 'NONE',  ( 17.69737658530999980, -0.08473977435852000917, -10.25642497589999991 ) ) ;
#13600 = EDGE_LOOP ( 'NONE', ( #18922, #246, #2189, #15387, #5707 ) ) ;
#13601 = B_SPLINE_CURVE_WITH_KNOTS ( 'NONE', 3,
 ( #21075, #23119, #4487, #2922, #475, #22999, #13802, #6417, #965, #8364, #1586, #19635, #3045, #10790, #5104, #15969, #16338, #1217, #23729, #14174, #16093, #8608, #21692, #4984, #14411, #1463, #8857, #7134, #6659, #14525, #10432, #21917, #14053, #5331, #17822, #21574, #12371, #3408, #12248, #17695 ),
 .UNSPECIFIED., .F., .F.,
 ( 4, 2, 2, 1, 2, 2, 2, 2, 1, 1, 2, 2, 2, 2, 2, 2, 2, 2, 1, 2, 2, 4 ),
 ( 0.000000000000000000, 0.1249999999999819311, 0.1874999999999721334, 0.2187499999999676370, 0.2343749999999661382, 0.2499999999999646394, 0.3749999999999477085, 0.4374999999999382161, 0.4687499999999327205, 0.4843749999999300559, 0.4921874999999286682, 0.4999999999999273359, 0.5624999999999176215, 0.5937499999999141798, 0.6093749999999130695, 0.6249999999999118483, 0.6874999999999157341, 0.7187499999999187317, 0.7343749999999219513, 0.7421874999999236167, 0.7499999999999251710, 1.000000000000000000 ),
 .UNSPECIFIED. ) ;
#13602 = CARTESIAN_POINT ( 'NONE',  ( 18.22028936713000036, -1.652712406954000013, 8.988165862088999702 ) ) ;
#13603 = CARTESIAN_POINT ( 'NONE',  ( -1.346439123299411733, 24.53198827073828880, -3.841100253456362523 ) ) ;
#13604 = CARTESIAN_POINT ( 'NONE',  ( 0.6124999999999999334, 1.217145837503000065E-14, 0.000000000000000000 ) ) ;
#13605 = EDGE_LOOP ( 'NONE', ( #14888, #6168, #5908, #10995 ) ) ;
#13606 = CARTESIAN_POINT ( 'NONE',  ( 3.999999999999999112, 26.41068681084913194, -1.228746328088897721 ) ) ;
#13607 = LINE ( 'NONE', #4416, #4332 ) ;
#13608 = CARTESIAN_POINT ( 'NONE',  ( 23.97064348353488228, 8.656922289499620504, 6.324528327562126684 ) ) ;
#13609 = CARTESIAN_POINT ( 'NONE',  ( 19.52828936713000019, 9.172416106433001204, 0.000000000000000000 ) ) ;
#13610 = CARTESIAN_POINT ( 'NONE',  ( 17.66745306301536544, -10.34082436438601427, -1.123769564641571295 ) ) ;
#13611 = CARTESIAN_POINT ( 'NONE',  ( 2.500000000000000000, 27.03419673618999752, 0.000000000000000000 ) ) ;
#13612 = CARTESIAN_POINT ( 'NONE',  ( -14.42499036736162843, 9.146326703434647598, -9.158041868011997266 ) ) ;
#13613 = CARTESIAN_POINT ( 'NONE',  ( -5.470519282017996865, 16.57663645147999532, -3.044056508385000193 ) ) ;
#13614 = CARTESIAN_POINT ( 'NONE',  ( 11.99999999337999945, 7.499999993379000252, 2.839929970532000182E-09 ) ) ;
#13615 = CARTESIAN_POINT ( 'NONE',  ( -0.6543697108982035049, 28.86753006952333678, -2.434931691670788823 ) ) ;
#13616 = FACE_OUTER_BOUND ( 'NONE', #16826, .T. ) ;
#13617 = CARTESIAN_POINT ( 'NONE',  ( -0.2706287508702177047, 30.38790270302602892, 2.145884556181206548 ) ) ;
#13618 = VERTEX_POINT ( 'NONE', #19141 ) ;
#13619 = CARTESIAN_POINT ( 'NONE',  ( -17.12799577250666516, 4.588264514863035437, 7.960958945508470386 ) ) ;
#13620 = CARTESIAN_POINT ( 'NONE',  ( 18.29451526988999888, 2.173595297473000176, 9.280136552624998814 ) ) ;
#13621 = CARTESIAN_POINT ( 'NONE',  ( -4.400811355473761566, 13.44820252045024844, -5.243297503433447915 ) ) ;
#13622 = CARTESIAN_POINT ( 'NONE',  ( 0.000000000000000000, 29.69999999999999929, 4.618802153517000519 ) ) ;
#13623 = ADVANCED_FACE ( 'NONE', ( #22535, #4132 ), #371, .F. ) ;
#13624 = CARTESIAN_POINT ( 'NONE',  ( -19.54644303974366082, -5.739935299888772491, 8.770143196517862449 ) ) ;
#13625 = CARTESIAN_POINT ( 'NONE',  ( -1.873164014766999896, 26.73196440325999745, -1.599833206071999969 ) ) ;
#13626 = TOROIDAL_SURFACE ( 'NONE', #3221, 2.100000000000000089, 0.1000000000000000056 ) ;
#13627 = CARTESIAN_POINT ( 'NONE',  ( -1.350644574833474776, 28.02555747447238943, 3.839035148322985425 ) ) ;
#13628 = ORIENTED_EDGE ( 'NONE', *, *, #7937, .T. ) ;
#13629 = CARTESIAN_POINT ( 'NONE',  ( -16.98657998867568253, 0.2181174425927162597, -10.41649861509676356 ) ) ;
#13630 = CARTESIAN_POINT ( 'NONE',  ( 0.000000000000000000, 15.00000000000000000, 0.000000000000000000 ) ) ;
#13631 = CARTESIAN_POINT ( 'NONE',  ( -0.9079114435473193412, 28.28457205800976126, -1.972232025669313105 ) ) ;
#13632 = EDGE_LOOP ( 'NONE', ( #21331, #12012, #15785, #5097, #6796 ) ) ;
#13633 = EDGE_CURVE ( 'NONE', #20779, #15215, #4393, .T. ) ;
#13634 = ORIENTED_EDGE ( 'NONE', *, *, #22280, .T. ) ;
#13635 = DIRECTION ( 'NONE',  ( 0.000000000000000000, -1.000000000000000000, 0.000000000000000000 ) ) ;
#13636 = CARTESIAN_POINT ( 'NONE',  ( 18.93037674931000325, -2.874963284959999754, 10.40852167983000065 ) ) ;
#13637 = CARTESIAN_POINT ( 'NONE',  ( -19.45545303391000047, -10.54334799148000101, 1.955063380522000127 ) ) ;
#13638 = CARTESIAN_POINT ( 'NONE',  ( -19.89493079071000281, -7.185997981995999595, 7.042515753137999823 ) ) ;
#13639 = FACE_BOUND ( 'NONE', #9788, .T. ) ;
#13640 = CARTESIAN_POINT ( 'NONE',  ( 16.07233580085999947, -5.589751863050000047, -9.898928778229000969 ) ) ;
#13641 = DIRECTION ( 'NONE',  ( 0.000000000000000000, -1.000000000000000000, 0.000000000000000000 ) ) ;
#13642 = VECTOR ( 'NONE', #20971, 1000.000000000000000 ) ;
#13643 = PLANE ( 'NONE',  #18390 ) ;
#13644 = CARTESIAN_POINT ( 'NONE',  ( 19.95901395809000078, -10.16568956861999951, -0.7466314648695999701 ) ) ;
#13645 = B_SPLINE_SURFACE_WITH_KNOTS ( 'NONE', 3, 3, ( 
 ( #4219, #6144, #18869, #11611, #14983, #22494, #5903 ),
 ( #13533, #4096, #2042, #2274, #6022, #11374, #20809 ),
 ( #17048, #328, #18745, #22730, #7733, #9548, #9432 ),
 ( #15465, #562, #16926, #9903, #15098, #5793, #16803 ) ),
 .UNSPECIFIED., .F., .F., .F.,
 ( 4, 4 ),
 ( 4, 1, 1, 1, 4 ),
 ( 0.5752948794218999407, 1.078423528826000011 ),
 ( 0.9199548376994000076, 0.9403585065211000904, 0.9607621753428000622, 0.9811658441645999540, 1.001569512986000055 ),
 .UNSPECIFIED. ) ;
#13646 = DIRECTION ( 'NONE',  ( 1.184237892933000067E-14, 1.000000000000000000, 2.412884706852000360E-14 ) ) ;
#13647 = VERTEX_POINT ( 'NONE', #9587 ) ;
#13648 = CARTESIAN_POINT ( 'NONE',  ( -12.50000000000000000, 6.606768802097000126, -6.099810110451000966 ) ) ;
#13649 = CARTESIAN_POINT ( 'NONE',  ( -0.6741018852137999895, 26.18706776952000226, -2.583184600869000036 ) ) ;
#13650 = CARTESIAN_POINT ( 'NONE',  ( 4.778589274750996374, 12.47906568194001764, 0.2464885544182001953 ) ) ;
#13651 = CARTESIAN_POINT ( 'NONE',  ( 2.070949786996742148, 28.96702299132843805, 0.6137957092266852488 ) ) ;
#13652 = EDGE_CURVE ( 'NONE', #23649, #8084, #13909, .T. ) ;
#13653 = CARTESIAN_POINT ( 'NONE',  ( -20.93315459384999855, -5.137598072637000080, -9.812497494458000347 ) ) ;
#13654 = ORIENTED_EDGE ( 'NONE', *, *, #9318, .T. ) ;
#13655 = DIRECTION ( 'NONE',  ( 1.000000000000000000, 0.000000000000000000, 0.000000000000000000 ) ) ;
#13656 = ORIENTED_EDGE ( 'NONE', *, *, #4685, .T. ) ;
#13657 = DIRECTION ( 'NONE',  ( 0.000000000000000000, -1.000000000000000000, 0.000000000000000000 ) ) ;
#13658 = CARTESIAN_POINT ( 'NONE',  ( -11.00000000000000000, -10.59999999999999964, 0.000000000000000000 ) ) ;
#13659 = CARTESIAN_POINT ( 'NONE',  ( -4.023597209795000573, 13.98887489068000356, 4.533200346611999443 ) ) ;
#13660 = PRODUCT_DEFINITION_FORMATION_WITH_SPECIFIED_SOURCE ( 'ANY', '', #11128, .NOT_KNOWN. ) ;
#13661 = CARTESIAN_POINT ( 'NONE',  ( -1.670944742899670432, 6.980577527795076342, 0.5248963117445855087 ) ) ;
#13662 = CARTESIAN_POINT ( 'NONE',  ( -1.200923599098000061, 28.00000000000000000, 5.906307787036999990 ) ) ;
#13663 = ADVANCED_FACE ( 'NONE', ( #5941 ), #13327, .F. ) ;
#13664 = CIRCLE ( 'NONE', #22948, 4.649999999999999467 ) ;
#13665 = CARTESIAN_POINT ( 'NONE',  ( -14.78308928803000022, -1.400056168502999965, -10.15245659134999912 ) ) ;
#13666 = CARTESIAN_POINT ( 'NONE',  ( 16.21856375731000099, 2.595497835609000159, 8.825947828509001170 ) ) ;
#13667 = CARTESIAN_POINT ( 'NONE',  ( 24.40278699097224901, 2.659935282767430298, 12.50000000000000000 ) ) ;
#13668 = ORIENTED_EDGE ( 'NONE', *, *, #10409, .T. ) ;
#13669 = CARTESIAN_POINT ( 'NONE',  ( 19.67611389298096114, -1.127737984101849555, -10.44857563443030557 ) ) ;
#13670 = CARTESIAN_POINT ( 'NONE',  ( 12.50000000000000000, -13.93375672974000068, 0.000000000000000000 ) ) ;
#13671 = CARTESIAN_POINT ( 'NONE',  ( -2.445536200447000041, 23.49107026052999814, 0.2165401555166999725 ) ) ;
#13672 = CARTESIAN_POINT ( 'NONE',  ( 4.036236897996232642, 14.47342755007821147, -4.607006349117426680 ) ) ;
#13673 = ORIENTED_EDGE ( 'NONE', *, *, #13530, .F. ) ;
#13674 = CARTESIAN_POINT ( 'NONE',  ( 0.000000000000000000, 28.30000000000000071, 4.618802153517000519 ) ) ;
#13675 = CARTESIAN_POINT ( 'NONE',  ( -24.24003052284538029, 12.62002563675921962, -3.141177558926625313 ) ) ;
#13676 = DIRECTION ( 'NONE',  ( 1.000000000000000000, 0.000000000000000000, 0.000000000000000000 ) ) ;
#13677 = CARTESIAN_POINT ( 'NONE',  ( -12.50000000000000000, 1.554281285377000029E-14, -7.500000000000916600 ) ) ;
#13678 = CARTESIAN_POINT ( 'NONE',  ( 17.62590205330530679, -8.442047657051244158, -6.393466172490128940 ) ) ;
#13679 = CARTESIAN_POINT ( 'NONE',  ( 2.500000000000000000, 29.19999999999999929, 0.000000000000000000 ) ) ;
#13680 = CIRCLE ( 'NONE', #16771, 1.500000000000000000 ) ;
#13681 = ADVANCED_FACE ( 'NONE', ( #2435 ), #23089, .F. ) ;
#13682 = SHAPE_REPRESENTATION ( 'MAS-673', ( #5168, #9030, #2054, #10964, #10187, #14440, #23714, #13268 ), #19476 ) ;
#13683 = EDGE_LOOP ( 'NONE', ( #845, #22121, #7426, #17313, #5213 ) ) ;
#13684 = CARTESIAN_POINT ( 'NONE',  ( -7.034000000000000696, 1.310788454998999989E-14, 0.000000000000000000 ) ) ;
#13685 = EDGE_CURVE ( 'NONE', #16101, #15884, #6853, .T. ) ;
#13686 = CARTESIAN_POINT ( 'NONE',  ( 11.40904387243762663, -9.351110459859503621, 8.803306989946506178 ) ) ;
#13687 = ORIENTED_EDGE ( 'NONE', *, *, #17020, .F. ) ;
#13688 = CARTESIAN_POINT ( 'NONE',  ( 0.000000000000000000, 26.35000000000000142, 4.309401076758999416 ) ) ;
#13689 = CARTESIAN_POINT ( 'NONE',  ( -6.000000000000000000, 26.50000000000000000, -6.000000000000000000 ) ) ;
#13690 = CARTESIAN_POINT ( 'NONE',  ( 2.689850711658643867, 13.04840579188256200, 6.170289802015100022 ) ) ;
#13691 = TOROIDAL_SURFACE ( 'NONE', #16779, 2.100000000000000089, 0.1000000000000000056 ) ;
#13692 = VECTOR ( 'NONE', #6093, 1000.000000000000114 ) ;
#13693 = CARTESIAN_POINT ( 'NONE',  ( 6.141454963614990881, 14.19352208129948956, -0.05101708110013205427 ) ) ;
#13694 = CARTESIAN_POINT ( 'NONE',  ( -20.58689978330333759, -0.5797656323877646845, 9.243770522370594378 ) ) ;
#13695 = CARTESIAN_POINT ( 'NONE',  ( 2.030158388880999976, 26.87419433610000397, 2.030158388880999976 ) ) ;
#13696 = EDGE_CURVE ( 'NONE', #4476, #20167, #4707, .T. ) ;
#13697 = VERTEX_POINT ( 'NONE', #16971 ) ;
#13698 = EDGE_LOOP ( 'NONE', ( #23158, #8626, #5766, #11231, #19877, #16589 ) ) ;
#13699 = EDGE_CURVE ( 'NONE', #5650, #4259, #15353, .T. ) ;
#13700 = CARTESIAN_POINT ( 'NONE',  ( -23.74465998031000069, 7.716878364870000340, -11.63397459621999985 ) ) ;
#13701 = CARTESIAN_POINT ( 'NONE',  ( 3.316026328257057010, 24.63336607546882817, 2.704152903937933061 ) ) ;
#13702 = DIRECTION ( 'NONE',  ( -0.7071067811823850136, -0.7071067811898851252, -1.080116769369976149E-06 ) ) ;
#13703 = ORIENTED_EDGE ( 'NONE', *, *, #5131, .F. ) ;
#13704 = CARTESIAN_POINT ( 'NONE',  ( 23.01485185659291233, 35.51856778792605240, -2.673746900119611247 ) ) ;
#13705 = CARTESIAN_POINT ( 'NONE',  ( 6.157250470212304982, 14.08721296600253403, 0.3655245610725118000 ) ) ;
#13706 = CARTESIAN_POINT ( 'NONE',  ( 15.88689183704831898, -10.11250081917797949, -2.234254655284192648 ) ) ;
#13707 = CARTESIAN_POINT ( 'NONE',  ( -18.52537075707000014, 9.692839761673001320, 5.440148519787000758 ) ) ;
#13708 = CARTESIAN_POINT ( 'NONE',  ( 0.6836813991273753555, 24.62756664670378015, 4.224074002598932509 ) ) ;
#13709 = CARTESIAN_POINT ( 'NONE',  ( -19.76373237314461306, -5.167322758071764888, 9.127427723831647910 ) ) ;
#13710 = CARTESIAN_POINT ( 'NONE',  ( -24.24721944463121304, -7.815463711320101758, -6.401738435092275026 ) ) ;
#13711 = CARTESIAN_POINT ( 'NONE',  ( -1.688436697687023758, 29.48963661612821596, 1.350056256019540157 ) ) ;
#13712 = ORIENTED_EDGE ( 'NONE', *, *, #23639, .T. ) ;
#13713 = CARTESIAN_POINT ( 'NONE',  ( 2.274201110986000085, 23.98977050234999808, 0.5876087361756999750 ) ) ;
#13714 = VECTOR ( 'NONE', #1020, 1000.000000000000000 ) ;
#13715 = CARTESIAN_POINT ( 'NONE',  ( -16.74920940442816075, 10.40545465073398645, -0.4181688731950466420 ) ) ;
#13716 = VERTEX_POINT ( 'NONE', #15026 ) ;
#13717 = FACE_OUTER_BOUND ( 'NONE', #19015, .T. ) ;
#13718 = CARTESIAN_POINT ( 'NONE',  ( 6.273195954926005236, 13.70238338811998702, -0.1819524851944001598 ) ) ;
#13719 = CARTESIAN_POINT ( 'NONE',  ( 12.00000000000000000, 3.342026269744088562, -8.334540845168532996 ) ) ;
#13720 = AXIS2_PLACEMENT_3D ( 'NONE', #9964, #754, #1495 ) ;
#13721 = FACE_OUTER_BOUND ( 'NONE', #21733, .T. ) ;
#13722 = CARTESIAN_POINT ( 'NONE',  ( 12.18656392131000210, 5.460236994095999385, -7.899338765649998706 ) ) ;
#13723 = ORIENTED_EDGE ( 'NONE', *, *, #14008, .F. ) ;
#13724 = CARTESIAN_POINT ( 'NONE',  ( 18.58787270046333262, -9.148283161302634525, 1.058975758512214815 ) ) ;
#13725 = CARTESIAN_POINT ( 'NONE',  ( -4.000000000000000000, 29.69999999999999929, 2.309401076759000304 ) ) ;
#13726 = DIRECTION ( 'NONE',  ( -1.000000000000000000, 0.000000000000000000, 0.000000000000000000 ) ) ;
#13727 = ORIENTED_EDGE ( 'NONE', *, *, #9120, .T. ) ;
#13728 = CARTESIAN_POINT ( 'NONE',  ( -1.382592897918908825, 24.72515053741216562, 1.690066663980638983 ) ) ;
#13729 = DIRECTION ( 'NONE',  ( 0.000000000000000000, -1.000000000000000000, 0.000000000000000000 ) ) ;
#13730 = DIRECTION ( 'NONE',  ( 1.000000000000000000, 0.000000000000000000, 0.000000000000000000 ) ) ;
#13731 = CONICAL_SURFACE ( 'NONE', #2514, 7.249999994591000529, 0.7853981633972997312 ) ;
#13732 = CARTESIAN_POINT ( 'NONE',  ( 4.000000000000000888, 26.44682129341587995, 0.9440428258623110302 ) ) ;
#13733 = CARTESIAN_POINT ( 'NONE',  ( 18.35290878106735946, 8.176867920054682770, -6.464955659164507651 ) ) ;
#13734 = DIRECTION ( 'NONE',  ( 0.000000000000000000, -1.000000000000000000, 0.000000000000000000 ) ) ;
#13735 = CARTESIAN_POINT ( 'NONE',  ( -14.25243324638999809, -7.716878364870000340, 11.63397459621999985 ) ) ;
#13736 = CARTESIAN_POINT ( 'NONE',  ( 21.92332918976000045, 10.92587188921000063, 2.656753488603999624 ) ) ;
#13737 = LINE ( 'NONE', #4304, #10470 ) ;
#13738 = CARTESIAN_POINT ( 'NONE',  ( -8.099999999999999645, -9.651424765286998664, -1.370599189697999991E-09 ) ) ;
#13739 = CARTESIAN_POINT ( 'NONE',  ( -2.147910637137995682, 30.21755022053942241, 0.2331351799471601260 ) ) ;
#13740 = VERTEX_POINT ( 'NONE', #13215 ) ;
#13741 = CARTESIAN_POINT ( 'NONE',  ( 18.54032793388999778, 2.288377001679999800, 9.770195530030999720 ) ) ;
#13742 = CARTESIAN_POINT ( 'NONE',  ( 2.011763616992924941, 12.94111840506035271, -6.392243311745070322 ) ) ;
#13743 = CARTESIAN_POINT ( 'NONE',  ( 1.259047450927257339, 27.70086340285666893, 2.184465970885639763 ) ) ;
#13744 = CARTESIAN_POINT ( 'NONE',  ( -20.59072166554749828, 1.091684521857474444, -10.45463456709096661 ) ) ;
#13745 = AXIS2_PLACEMENT_3D ( 'NONE', #12174, #8547, #13981 ) ;
#13746 = DIRECTION ( 'NONE',  ( 0.000000000000000000, 1.000000000000000000, 0.000000000000000000 ) ) ;
#13747 = VECTOR ( 'NONE', #8732, 1000.000000000000114 ) ;
#13748 = DIRECTION ( 'NONE',  ( 0.000000000000000000, 1.000000000000000000, 0.000000000000000000 ) ) ;
#13749 = ORIENTED_EDGE ( 'NONE', *, *, #9479, .F. ) ;
#13750 = CARTESIAN_POINT ( 'NONE',  ( -16.73537885361223232, 8.099390186838867578, -6.548858784556899515 ) ) ;
#13751 = CARTESIAN_POINT ( 'NONE',  ( 0.5458742448588185248, 26.26180390196785908, 2.091772243866166114 ) ) ;
#13752 = CARTESIAN_POINT ( 'NONE',  ( -2.089563112090822017, 27.66818174792411611, 0.6513645842518486218 ) ) ;
#13753 = ORIENTED_EDGE ( 'NONE', *, *, #3936, .F. ) ;
#13754 = ORIENTED_EDGE ( 'NONE', *, *, #21636, .T. ) ;
#13755 = CARTESIAN_POINT ( 'NONE',  ( 24.19085492956958561, -9.549256642876626344, 0.0002501093553063627687 ) ) ;
#13756 = CARTESIAN_POINT ( 'NONE',  ( 18.38193924931000112, 10.76489784149000251, -0.6396482201651000343 ) ) ;
#13757 = CARTESIAN_POINT ( 'NONE',  ( -14.38421993232999085, -3.906483176905686694, -8.205166477479426845 ) ) ;
#13758 = EDGE_CURVE ( 'NONE', #23625, #16342, #4264, .T. ) ;
#13759 = CARTESIAN_POINT ( 'NONE',  ( -14.81667209146000097, 4.829413564942999670, 9.643273172525999470 ) ) ;
#13760 = CARTESIAN_POINT ( 'NONE',  ( 22.49408333333332521, 2.420664364967175075, -9.007858475302045420 ) ) ;
#13761 = CARTESIAN_POINT ( 'NONE',  ( 18.91749951746000136, 2.321179906104000157, -9.550167091796001984 ) ) ;
#13762 = CARTESIAN_POINT ( 'NONE',  ( 2.063594504837999888E-14, 28.80370090847999975, 2.160000000000000142 ) ) ;
#13763 = AXIS2_PLACEMENT_3D ( 'NONE', #161, #4164, #11558 ) ;
#13764 = CARTESIAN_POINT ( 'NONE',  ( 0.3272492347489454056, 26.85086340285666751, 2.499999999999998668 ) ) ;
#13765 = CARTESIAN_POINT ( 'NONE',  ( 22.79179959256000387, 9.200607065852999256, 4.564250555339000037 ) ) ;
#13766 = CARTESIAN_POINT ( 'NONE',  ( 0.000000000000000000, 14.95000002005000006, 0.000000000000000000 ) ) ;
#13767 = EDGE_LOOP ( 'NONE', ( #12954, #16999, #12697, #16903 ) ) ;
#13768 = CARTESIAN_POINT ( 'NONE',  ( -0.5828398938954729713, 13.70670201154066348, 6.100149040538799916 ) ) ;
#13769 = CARTESIAN_POINT ( 'NONE',  ( 0.5047246425491000998, 26.68250240009999885, 2.826365205286999860 ) ) ;
#13770 = AXIS2_PLACEMENT_3D ( 'NONE', #11566, #18944, #4535 ) ;
#13771 = CARTESIAN_POINT ( 'NONE',  ( -4.720280981314001423, 12.53503187393000751, -0.1499689402456999276 ) ) ;
#13772 = CARTESIAN_POINT ( 'NONE',  ( 0.8066938640923024817, 28.85226775220604623, 2.013103552383532335 ) ) ;
#13773 = EDGE_CURVE ( 'NONE', #22774, #6663, #21735, .T. ) ;
#13774 = CARTESIAN_POINT ( 'NONE',  ( -24.25438256056000341, 9.890429046451000517, -5.183062093339000143 ) ) ;
#13775 = LINE ( 'NONE', #8338, #13091 ) ;
#13776 = VERTEX_POINT ( 'NONE', #17329 ) ;
#13777 = CARTESIAN_POINT ( 'NONE',  ( 15.40899770046332051, -1.186956113863760320, -9.066706963569007627 ) ) ;
#13778 = CARTESIAN_POINT ( 'NONE',  ( -7.500000000000000000, -10.00000000000000000, 0.000000000000000000 ) ) ;
#13779 = CARTESIAN_POINT ( 'NONE',  ( -2.386616373980000372, 14.08111751881002327, 5.671222873807000298 ) ) ;
#13780 = TOROIDAL_SURFACE ( 'NONE', #21904, 10.50000000000000000, 0.1000000000000000056 ) ;
#13781 = CARTESIAN_POINT ( 'NONE',  ( 1.215150159706073874, 6.885362815765219580, 1.263354467349552701 ) ) ;
#13782 = CARTESIAN_POINT ( 'NONE',  ( 13.50000000000000000, 0.000000000000000000, 0.000000000000000000 ) ) ;
#13783 = CARTESIAN_POINT ( 'NONE',  ( -0.6543697108982035049, 27.26753006952333891, -2.434931691670788823 ) ) ;
#13784 = CARTESIAN_POINT ( 'NONE',  ( -13.84895371062999914, -11.26122607477999971, -0.8537354506236000118 ) ) ;
#13785 = CARTESIAN_POINT ( 'NONE',  ( 12.81825125731000092, -4.388733341911000174, 7.983506680731000671 ) ) ;
#13786 = CARTESIAN_POINT ( 'NONE',  ( 23.99062354302999722, 6.216878364870000340, 12.50000000000000000 ) ) ;
#13787 = ADVANCED_FACE ( 'NONE', ( #6791 ), #18092, .T. ) ;
#13788 = ORIENTED_EDGE ( 'NONE', *, *, #22451, .F. ) ;
#13789 = CARTESIAN_POINT ( 'NONE',  ( -2.434931691670790155, 28.76666666666667282, -0.6543697108981958444 ) ) ;
#13790 = CARTESIAN_POINT ( 'NONE',  ( 1.066440661507000121, 30.89923340193000101, -2.297374585629999633 ) ) ;
#13791 = CIRCLE ( 'NONE', #16108, 1.000000757558000553 ) ;
#13792 = CARTESIAN_POINT ( 'NONE',  ( -2.596050696748999798, 23.36428859183000029, -0.2023800179719000003 ) ) ;
#13793 = CARTESIAN_POINT ( 'NONE',  ( 3.076789502295112833, 14.15080769385439652, -5.296133739446251099 ) ) ;
#13794 = ORIENTED_EDGE ( 'NONE', *, *, #20978, .T. ) ;
#13795 = AXIS2_PLACEMENT_3D ( 'NONE', #13072, #22396, #22162 ) ;
#13796 = DIRECTION ( 'NONE',  ( 1.000000000000000000, 0.000000000000000000, 0.000000000000000000 ) ) ;
#13797 = PLANE ( 'NONE',  #16973 ) ;
#13798 = DIRECTION ( 'NONE',  ( 1.000000000000000000, 0.000000000000000000, 0.000000000000000000 ) ) ;
#13799 = CARTESIAN_POINT ( 'NONE',  ( 11.32654380050958309, 2.569587902822825232, 12.49997024370573939 ) ) ;
#13800 = CARTESIAN_POINT ( 'NONE',  ( 16.78958611615448149, 6.561663190455382377, 8.105752677713512711 ) ) ;
#13801 = AXIS2_PLACEMENT_3D ( 'NONE', #9326, #16463, #20470 ) ;
#13802 = CARTESIAN_POINT ( 'NONE',  ( -4.348907022798502275, 13.58078079707876995, 4.987290125177318956 ) ) ;
#13803 = CARTESIAN_POINT ( 'NONE',  ( -21.47403743917331909, 1.207329456531927248, -9.222347836830195433 ) ) ;
#13804 = ADVANCED_FACE ( 'NONE', ( #2810 ), #8422, .T. ) ;
#13805 = CARTESIAN_POINT ( 'NONE',  ( 24.40278699097225612, -12.15528518867914620, -3.946428472716975833 ) ) ;
#13806 = ORIENTED_EDGE ( 'NONE', *, *, #21675, .F. ) ;
#13807 = CARTESIAN_POINT ( 'NONE',  ( 0.000000000000000000, 19.00000000000000000, -2.899999999999999911 ) ) ;
#13808 = CARTESIAN_POINT ( 'NONE',  ( 11.07373617190885184, -10.57520287780550206, 6.683140124596108400 ) ) ;
#13809 = ORIENTED_EDGE ( 'NONE', *, *, #3934, .T. ) ;
#13810 = CARTESIAN_POINT ( 'NONE',  ( -14.25243324638999809, 6.216878364870000340, -12.50000000000000000 ) ) ;
#13811 = CARTESIAN_POINT ( 'NONE',  ( 0.2737217042541190692, 24.02003154414986597, 2.176099354324680490 ) ) ;
#13812 = CARTESIAN_POINT ( 'NONE',  ( 4.133705205700141327, 13.37470319316354406, 5.426825399075087653 ) ) ;
#13813 = AXIS2_PLACEMENT_3D ( 'NONE', #18528, #222, #18880 ) ;
#13814 = CARTESIAN_POINT ( 'NONE',  ( 6.150813686940276526, 14.12672329618388467, -0.2685225048143122795 ) ) ;
#13815 = CARTESIAN_POINT ( 'NONE',  ( -6.454293914649997355, 15.34141787428001180, -0.9747575175365998934 ) ) ;
#13816 = EDGE_CURVE ( 'NONE', #20493, #17324, #21563, .T. ) ;
#13817 = DIRECTION ( 'NONE',  ( 0.000000000000000000, 0.000000000000000000, 1.000000000000000000 ) ) ;
#13818 = ORIENTED_EDGE ( 'NONE', *, *, #1722, .F. ) ;
#13819 = CIRCLE ( 'NONE', #3406, 4.649999999999999467 ) ;
#13820 = ORIENTED_EDGE ( 'NONE', *, *, #8147, .T. ) ;
#13821 = CARTESIAN_POINT ( 'NONE',  ( 2.434931691670791487, 30.20086340285667958, 0.6543697108981911814 ) ) ;
#13822 = CARTESIAN_POINT ( 'NONE',  ( -0.05078100571018644843, 26.49647344481827815, -2.396473444817840637 ) ) ;
#13823 = CARTESIAN_POINT ( 'NONE',  ( 0.000000000000000000, 16.94999982584599962, 0.000000000000000000 ) ) ;
#13824 = EDGE_CURVE ( 'NONE', #17699, #12075, #16233, .T. ) ;
#13825 = AXIS2_PLACEMENT_3D ( 'NONE', #676, #8083, #15567 ) ;
#13826 = ORIENTED_EDGE ( 'NONE', *, *, #2587, .F. ) ;
#13827 = EDGE_CURVE ( 'NONE', #17905, #11381, #21165, .T. ) ;
#13828 = CARTESIAN_POINT ( 'NONE',  ( 2.164939593608602220, 27.99999999999984368, -3.368873696368142490 ) ) ;
#13829 = CARTESIAN_POINT ( 'NONE',  ( 24.00034722001000276, 7.216970193741999218, -11.92259671338999993 ) ) ;
#13830 = CARTESIAN_POINT ( 'NONE',  ( 14.98923988655635497, 9.998246065564853069, 2.609326537872780793 ) ) ;
#13831 = CARTESIAN_POINT ( 'NONE',  ( -15.09276777146999926, 10.87078250371000010, -1.814120968959000102 ) ) ;
#13832 = CARTESIAN_POINT ( 'NONE',  ( -20.35564026534377291, 10.49329004425314693, 0.3800888360172406943 ) ) ;
#13833 = CARTESIAN_POINT ( 'NONE',  ( -4.588558270747998158, 12.55560619728998972, -1.211727637559999904 ) ) ;
#13834 = AXIS2_PLACEMENT_3D ( 'NONE', #344, #5687, #13073 ) ;
#13835 = CARTESIAN_POINT ( 'NONE',  ( -24.37360972231626377, -9.140674791923824927, -4.597026942064932342 ) ) ;
#13836 = CARTESIAN_POINT ( 'NONE',  ( -1.095779270870209654, 29.53601415047671352, 1.861248250499890844 ) ) ;
#13837 = EDGE_CURVE ( 'NONE', #3316, #17036, #7259, .T. ) ;
#13838 = ORIENTED_EDGE ( 'NONE', *, *, #18866, .T. ) ;
#13839 = CARTESIAN_POINT ( 'NONE',  ( 0.4183838372234000014, 24.19916379885000168, -2.311326400246999757 ) ) ;
#13840 = CARTESIAN_POINT ( 'NONE',  ( -15.09967649506999798, 8.662012103627256820, -5.976300280193180825 ) ) ;
#13841 = ORIENTED_EDGE ( 'NONE', *, *, #21994, .F. ) ;
#13842 = CARTESIAN_POINT ( 'NONE',  ( 6.037827715737003054, 14.51810667922999087, -1.086417744412999653 ) ) ;
#13843 = CARTESIAN_POINT ( 'NONE',  ( -4.701368215507619297, 13.42162485236267599, -5.311323292224679804 ) ) ;
#13844 = CARTESIAN_POINT ( 'NONE',  ( -24.50000000000000000, -0.9970802404058677348, -10.51200122757351174 ) ) ;
#13845 = CARTESIAN_POINT ( 'NONE',  ( 13.17375142130999954, -7.436937191241000278, 6.115943375764999246 ) ) ;
#13846 = EDGE_LOOP ( 'NONE', ( #8947, #19746, #18350, #21577, #7885 ) ) ;
#13847 = CARTESIAN_POINT ( 'NONE',  ( 1.346883420029665982E-05, 28.56481971072916792, 2.273192963938693190 ) ) ;
#13848 = CIRCLE ( 'NONE', #16941, 2.000000000000000000 ) ;
#13849 = FACE_OUTER_BOUND ( 'NONE', #17056, .T. ) ;
#13850 = CARTESIAN_POINT ( 'NONE',  ( 12.52688711657000020, 13.93375672974000068, 0.8660254037843999608 ) ) ;
#13851 = PRODUCT ( 'Ball Seat Ring', 'Ball Seat Ring', '', ( #6855 ) ) ;
#13852 = EDGE_LOOP ( 'NONE', ( #22621, #11981, #18905, #6982 ) ) ;
#13853 = CARTESIAN_POINT ( 'NONE',  ( -2.246347731941017223, 24.65365226805931087, -5.222125272214524731E-08 ) ) ;
#13854 = CARTESIAN_POINT ( 'NONE',  ( 21.36033333333333317, 4.643197203103720305, 8.055763831365723604 ) ) ;
#13855 = DIRECTION ( 'NONE',  ( 1.000000000000000000, 0.000000000000000000, 0.000000000000000000 ) ) ;
#13856 = CARTESIAN_POINT ( 'NONE',  ( -14.00000000000000355, -1.769624730688005076, 9.693260132994977241 ) ) ;
#13857 = CARTESIAN_POINT ( 'NONE',  ( 16.57009594051854506, 8.851926291245774792, -5.490978545969712243 ) ) ;
#13858 = DIRECTION ( 'NONE',  ( -1.000000000000000000, 0.000000000000000000, 0.000000000000000000 ) ) ;
#13859 = AXIS2_PLACEMENT_3D ( 'NONE', #13176, #17168, #13289 ) ;
#13860 = CARTESIAN_POINT ( 'NONE',  ( -14.33281102374372473, 13.40129170500425460, -1.788281879885584624 ) ) ;
#13861 = CARTESIAN_POINT ( 'NONE',  ( 22.80413863851999778, -10.54592076045000049, 3.969997482439000525 ) ) ;
#13862 = LINE ( 'NONE', #19192, #2466 ) ;
#13863 = AXIS2_PLACEMENT_3D ( 'NONE', #15064, #19854, #3270 ) ;
#13864 = B_SPLINE_CURVE_WITH_KNOTS ( 'NONE', 3,
 ( #16918, #17042, #440, #22608 ),
 .UNSPECIFIED., .F., .F.,
 ( 4, 4 ),
 ( 0.000000000000000000, 1.000000000000000000 ),
 .UNSPECIFIED. ) ;
#13865 = CARTESIAN_POINT ( 'NONE',  ( -3.830485454497844611, 14.04491027079380494, -4.850755123483903475 ) ) ;
#13866 = CARTESIAN_POINT ( 'NONE',  ( -5.833999999999999631, 1.296092693409999996E-14, 0.000000000000000000 ) ) ;
#13867 = CARTESIAN_POINT ( 'NONE',  ( -1.899230582703691272, 30.14058891630886450, -1.028631790195981388 ) ) ;
#13868 = EDGE_CURVE ( 'NONE', #20307, #21964, #1223, .T. ) ;
#13869 = EDGE_LOOP ( 'NONE', ( #21272, #33, #6733, #1959 ) ) ;
#13870 = CARTESIAN_POINT ( 'NONE',  ( 20.80677740615999838, -8.429461903092001052, -5.987368277389999882 ) ) ;
#13871 = CARTESIAN_POINT ( 'NONE',  ( 24.12965592620283672, 9.344095902241738472, 5.044035288470976042 ) ) ;
#13872 = CARTESIAN_POINT ( 'NONE',  ( 0.000000000000000000, 26.50000000000000355, 0.000000000000000000 ) ) ;
#13873 = AXIS2_PLACEMENT_3D ( 'NONE', #13903, #6153, #13540 ) ;
#13874 = CARTESIAN_POINT ( 'NONE',  ( -20.69782716562949432, -2.778284679047643646, -10.13681908816563926 ) ) ;
#13875 = DIRECTION ( 'NONE',  ( 0.000000000000000000, 1.000000000000000000, 0.000000000000000000 ) ) ;
#13876 = CARTESIAN_POINT ( 'NONE',  ( 4.829979889486999411, 12.47095937650998820, -1.110733291722999283 ) ) ;
#13877 = ORIENTED_EDGE ( 'NONE', *, *, #3336, .T. ) ;
#13878 = CIRCLE ( 'NONE', #5770, 2.750000000000000000 ) ;
#13879 = CARTESIAN_POINT ( 'NONE',  ( -16.23297658348885264, 5.081863263689504251, 9.076500965692741119 ) ) ;
#13880 = CARTESIAN_POINT ( 'NONE',  ( -5.833999999999999631, 11.50000000000000000, 0.000000000000000000 ) ) ;
#13881 = CARTESIAN_POINT ( 'NONE',  ( -0.8183426631040646715, 28.58043940685084294, 2.011287406255212851 ) ) ;
#13882 = CARTESIAN_POINT ( 'NONE',  ( 0.000000000000000000, 24.49999999999999645, 0.000000000000000000 ) ) ;
#13883 = EDGE_LOOP ( 'NONE', ( #16013, #2966, #15875, #23942 ) ) ;
#13884 = CARTESIAN_POINT ( 'NONE',  ( 17.18520603379667477, -2.385239382193358182, -8.875070924070865175 ) ) ;
#13885 = AXIS2_PLACEMENT_3D ( 'NONE', #5509, #8920, #1406 ) ;
#13886 = DIRECTION ( 'NONE',  ( 0.000000000000000000, 0.000000000000000000, -1.000000000000000000 ) ) ;
#13887 = CARTESIAN_POINT ( 'NONE',  ( -21.81072441343999913, 5.248549362552000552, 9.854325464458000283 ) ) ;
#13888 = CARTESIAN_POINT ( 'NONE',  ( -14.67959218088999940, -8.291367167875000277, 6.018862870213999905 ) ) ;
#13889 = CARTESIAN_POINT ( 'NONE',  ( -6.225556268444002228, 15.63956656239001575, 1.260315956371999446 ) ) ;
#13890 = CARTESIAN_POINT ( 'NONE',  ( 13.50083285078999928, 2.897491670606999747, -8.682224649056999866 ) ) ;
#13891 = CARTESIAN_POINT ( 'NONE',  ( -14.25699038479000080, -13.93375672974000068, 0.000000000000000000 ) ) ;
#13892 = CARTESIAN_POINT ( 'NONE',  ( -4.544324455327999779, 13.49053734526000170, 5.132126114358000812 ) ) ;
#13893 = AXIS2_PLACEMENT_3D ( 'NONE', #11296, #12978, #22647 ) ;
#13894 = DIRECTION ( 'NONE',  ( 0.000000000000000000, 0.000000000000000000, -1.000000000000000000 ) ) ;
#13895 = VERTEX_POINT ( 'NONE', #14534 ) ;
#13896 = CARTESIAN_POINT ( 'NONE',  ( -2.409957067094174565, 13.97492973469119448, 5.631351995472492433 ) ) ;
#13897 = CARTESIAN_POINT ( 'NONE',  ( -0.06321855798620600042, 24.77054417338800718, 2.143747832292392186 ) ) ;
#13898 = CIRCLE ( 'NONE', #9646, 4.549999999999999822 ) ;
#13899 = B_SPLINE_CURVE_WITH_KNOTS ( 'NONE', 3,
 ( #4640, #23518, #990, #15877, #21227, #23267, #18079, #8392 ),
 .UNSPECIFIED., .F., .F.,
 ( 4, 2, 2, 4 ),
 ( 0.000000000000000000, 0.2500000000000002220, 0.5000000000000004441, 1.000000000000000000 ),
 .UNSPECIFIED. ) ;
#13900 = CIRCLE ( 'NONE', #11976, 2.000000000000000000 ) ;
#13901 = CARTESIAN_POINT ( 'NONE',  ( 3.064125534931650296, 26.41068681084918524, 2.849728451093326953 ) ) ;
#13902 = CARTESIAN_POINT ( 'NONE',  ( -21.24686073652000218, -9.675487687114999957, -5.408659645178999220 ) ) ;
#13903 = CARTESIAN_POINT ( 'NONE',  ( -7.500000000000000000, 18.50000000000000000, -6.000000000000000000 ) ) ;
#13904 = ORIENTED_EDGE ( 'NONE', *, *, #2730, .T. ) ;
#13905 = ADVANCED_FACE ( 'NONE', ( #12728 ), #20234, .T. ) ;
#13906 = DIRECTION ( 'NONE',  ( 0.000000000000000000, 0.9997423213046380264, 0.02270002185933085032 ) ) ;
#13907 = CARTESIAN_POINT ( 'NONE',  ( 4.343596930150846802, 12.26443547612926110, -2.147542669209427491 ) ) ;
#13908 = FACE_OUTER_BOUND ( 'NONE', #19858, .T. ) ;
#13909 = B_SPLINE_CURVE_WITH_KNOTS ( 'NONE', 3,
 ( #2192, #14906, #2553, #22424, #7654, #20500, #6059, #2080 ),
 .UNSPECIFIED., .F., .F.,
 ( 4, 2, 2, 4 ),
 ( 0.000000000000000000, 0.2499999999999998890, 0.4999999999999997780, 1.000000000000000000 ),
 .UNSPECIFIED. ) ;
#13910 = CARTESIAN_POINT ( 'NONE',  ( -1.625770310270910901, 6.969985010803154246, 0.6506056477007011729 ) ) ;
#13911 = CARTESIAN_POINT ( 'NONE',  ( 0.000000000000000000, 17.95000004008999994, 0.000000000000000000 ) ) ;
#13912 = AXIS2_PLACEMENT_3D ( 'NONE', #21515, #13748, #8676 ) ;
#13913 = CARTESIAN_POINT ( 'NONE',  ( -9.377904711694998952, 11.69296112842000035, -10.27916260946000193 ) ) ;
#13914 = CARTESIAN_POINT ( 'NONE',  ( -6.062127672058159611, 16.18558825329198214, -1.005394117991464276 ) ) ;
#13915 = CARTESIAN_POINT ( 'NONE',  ( 15.12168875731000028, -7.425874990359000449, -5.381511109182000041 ) ) ;
#13916 = CARTESIAN_POINT ( 'NONE',  ( 19.00748459915545752, -0.3300499044338658927, 10.45037867241294371 ) ) ;
#13917 = ORIENTED_EDGE ( 'NONE', *, *, #14846, .F. ) ;
#13918 = CARTESIAN_POINT ( 'NONE',  ( 0.3272492347489343589, 28.58333333333333570, -2.500000000000000444 ) ) ;
#13919 = CARTESIAN_POINT ( 'NONE',  ( 1.580360580230000034, 29.84035787434000042, 1.979290453440999853 ) ) ;
#13920 = CARTESIAN_POINT ( 'NONE',  ( -15.42737077250666644, 7.250632197270348911, 5.572294543148784030 ) ) ;
#13921 = DIRECTION ( 'NONE',  ( 0.000000000000000000, -1.000000000000000000, 0.000000000000000000 ) ) ;
#13922 = AXIS2_PLACEMENT_3D ( 'NONE', #19627, #3035, #1209 ) ;
#13923 = ORIENTED_EDGE ( 'NONE', *, *, #14522, .T. ) ;
#13924 = FACE_BOUND ( 'NONE', #23308, .T. ) ;
#13925 = CARTESIAN_POINT ( 'NONE',  ( 0.000000000000000000, 13.00000000000000000, 0.000000000000000000 ) ) ;
#13926 = CARTESIAN_POINT ( 'NONE',  ( 0.5907988678278000005, 28.40181313824999876, 2.681278056231000129 ) ) ;
#13927 = CARTESIAN_POINT ( 'NONE',  ( -5.990165124597438329, 16.36624069022721528, 1.318159437083336272 ) ) ;
#13928 = CARTESIAN_POINT ( 'NONE',  ( 15.64662100204322215, -10.36655533400305274, -0.7640403907738141376 ) ) ;
#13929 = CARTESIAN_POINT ( 'NONE',  ( 0.000000000000000000, -1.550000000000000044, 0.000000000000000000 ) ) ;
#13930 = DIRECTION ( 'NONE',  ( 0.7071067811868960717, 0.7071067811861969643, 5.329912238617969693E-08 ) ) ;
#13931 = CARTESIAN_POINT ( 'NONE',  ( -11.04281598264000053, 1.359882291614000008E-14, 0.000000000000000000 ) ) ;
#13932 = ORIENTED_EDGE ( 'NONE', *, *, #9654, .F. ) ;
#13933 = CARTESIAN_POINT ( 'NONE',  ( -24.50000000000000000, -8.081477262649000792, -6.807253044743999837 ) ) ;
#13934 = CARTESIAN_POINT ( 'NONE',  ( 11.83261479513829784, -8.603276725215390996, 10.09871632141666176 ) ) ;
#13935 = ORIENTED_EDGE ( 'NONE', *, *, #13024, .F. ) ;
#13936 = B_SPLINE_CURVE_WITH_KNOTS ( 'NONE', 3,
 ( #14613, #16544, #2017, #23936, #14728, #20309, #3714, #11105, #22472, #19074, #5882, #8188, #11464, #2368, #9757, #13507, #2246, #13267, #9640, #17143, #15076, #17024, #2743, #21141, #11701, #15310, #423, #2489, #540, #20906, #13742, #21019, #11821, #11947, #7823, #4310, #4431, #20661, #2613, #18842, #6360, #4556, #20782, #15194, #19199, #4188, #22590, #4072, #7945, #22705, #6114, #17393, #10002, #13380, #9878, #17264, #5995, #11585, #663, #788, #7707, #18960, #19332, #15556, #22943, #8069, #10123, #22825, #300, #15438, #6239, #13621, #8668 ),
 .UNSPECIFIED., .F., .F.,
 ( 4, 2, 2, 1, 1, 1, 2, 2, 2, 2, 1, 1, 1, 2, 2, 2, 2, 1, 1, 2, 2, 2, 1, 1, 2, 2, 2, 1, 1, 1, 2, 2, 2, 2, 2, 2, 2, 2, 2, 2, 2, 2, 4 ),
 ( 0.000000000000000000, 0.06249999999999331091, 0.09374999999999010514, 0.1093749999999885647, 0.1171874999999877598, 0.1210937499999874684, 0.1230468749999873851, 0.1249999999999873157, 0.1874999999999849842, 0.2187499999999837907, 0.2343749999999832079, 0.2421874999999829026, 0.2460937499999827083, 0.2480468749999827915, 0.2499999999999828471, 0.3124999999999827915, 0.3437499999999828471, 0.3593749999999827915, 0.3671874999999826805, 0.3710937499999827915, 0.3749999999999828471, 0.4374999999999854006, 0.4687499999999866773, 0.4843749999999872879, 0.4921874999999875655, 0.4999999999999878986, 0.5624999999999898970, 0.5937499999999908962, 0.6093749999999914513, 0.6171874999999916733, 0.6210937499999917843, 0.6249999999999918954, 0.6874999999999938938, 0.7187499999999948930, 0.7499999999999958922, 0.8124999999999978906, 0.8203124999999980016, 0.8281249999999982236, 0.8437499999999984457, 0.8749999999999986677, 0.9062499999999990008, 0.9374999999999993339, 1.000000000000000000 ),
 .UNSPECIFIED. ) ;
#13937 = EDGE_CURVE ( 'NONE', #2137, #379, #8806, .T. ) ;
#13938 = CARTESIAN_POINT ( 'NONE',  ( -0.6531029714935000507, 25.61332603901999860, 2.260778022581000357 ) ) ;
#13939 = CARTESIAN_POINT ( 'NONE',  ( -6.637070260807000466, 26.50000000000000000, 2.000000000000000000 ) ) ;
#13940 = CARTESIAN_POINT ( 'NONE',  ( 0.6306621565982972744, 12.81494453417391810, 6.641634381469641468 ) ) ;
#13941 = CARTESIAN_POINT ( 'NONE',  ( 6.156111259623703091, 14.09394095567527572, -0.3492167251953930962 ) ) ;
#13942 = DIRECTION ( 'NONE',  ( 1.000000000000000000, 0.000000000000000000, 0.000000000000000000 ) ) ;
#13943 = CARTESIAN_POINT ( 'NONE',  ( 24.28255857084583624, -4.111234970449187287, -12.50000000000000533 ) ) ;
#13944 = ORIENTED_EDGE ( 'NONE', *, *, #22792, .T. ) ;
#13945 = DIRECTION ( 'NONE',  ( 0.000000000000000000, 1.000000000000000000, 0.000000000000000000 ) ) ;
#13946 = CARTESIAN_POINT ( 'NONE',  ( 0.000000000000000000, 22.00000000000000000, 0.000000000000000000 ) ) ;
#13947 = CARTESIAN_POINT ( 'NONE',  ( 0.000000000000000000, -14.43375672974000068, 0.000000000000000000 ) ) ;
#13948 = EDGE_LOOP ( 'NONE', ( #1400, #1416, #16154, #18877 ) ) ;
#13949 = ADVANCED_FACE ( 'NONE', ( #22268 ), #22624, .T. ) ;
#13950 = CARTESIAN_POINT ( 'NONE',  ( -23.17505693544000422, 0.9177324661394998806, 10.72000274858999980 ) ) ;
#13951 = CYLINDRICAL_SURFACE ( 'NONE', #18668, 10.65000000000000036 ) ;
#13952 = CARTESIAN_POINT ( 'NONE',  ( 20.33995833333332470, -7.351623071504412188, -5.649588876138436966 ) ) ;
#13953 = CARTESIAN_POINT ( 'NONE',  ( 15.07770949396983617, 8.779094814448228590, 5.457277787253644874 ) ) ;
#13954 = CARTESIAN_POINT ( 'NONE',  ( -14.76548285955000139, 9.865459827462000675, 4.892865777766999713 ) ) ;
#13955 = CARTESIAN_POINT ( 'NONE',  ( -4.000000000000000000, 24.80000000000000426, 2.309401076759000304 ) ) ;
#13956 = DIRECTION ( 'NONE',  ( 1.000000000000000000, 0.000000000000000000, 0.000000000000000000 ) ) ;
#13957 = CARTESIAN_POINT ( 'NONE',  ( 1.367099767897999918, 11.70857751387000434, -4.578439149374998962 ) ) ;
#13958 = PLANE ( 'NONE',  #2900 ) ;
#13959 = ADVANCED_FACE ( 'NONE', ( #14881 ), #10740, .T. ) ;
#13960 = CARTESIAN_POINT ( 'NONE',  ( -0.4927160651647209955, 29.57458059066297196, 2.103003212775674147 ) ) ;
#13961 = ORIENTED_EDGE ( 'NONE', *, *, #1439, .T. ) ;
#13962 = CARTESIAN_POINT ( 'NONE',  ( 2.500000000000000000, 29.21666666666666856, -0.3272492347489370235 ) ) ;
#13963 = CARTESIAN_POINT ( 'NONE',  ( -14.63664971349574273, 5.615217594154322533, 8.712278466216046624 ) ) ;
#13964 = B_SPLINE_CURVE_WITH_KNOTS ( 'NONE', 3,
 ( #652, #6103, #17626, #4301, #17751 ),
 .UNSPECIFIED., .F., .F.,
 ( 4, 1, 4 ),
 ( 0.000000000000000000, 0.5000000000000000000, 1.000000000000000000 ),
 .UNSPECIFIED. ) ;
#13965 = CONICAL_SURFACE ( 'NONE', #7774, 4.674999969225999585, 0.7853981633972997312 ) ;
#13966 = ORIENTED_EDGE ( 'NONE', *, *, #3324, .T. ) ;
#13967 = EDGE_CURVE ( 'NONE', #7090, #20281, #11109, .T. ) ;
#13968 = CARTESIAN_POINT ( 'NONE',  ( -23.76320767093000086, 6.967315680849999637, -12.06673481360999922 ) ) ;
#13969 = CARTESIAN_POINT ( 'NONE',  ( 5.100994270091002036, 14.04962196135000418, -3.662671701414000225 ) ) ;
#13970 = CARTESIAN_POINT ( 'NONE',  ( 12.00000000000000000, 0.9388500350608516287, -8.930124715774828914 ) ) ;
#13971 = CARTESIAN_POINT ( 'NONE',  ( 24.18393254356921318, 4.886968879241179842, -12.50000000000000000 ) ) ;
#13972 = CARTESIAN_POINT ( 'NONE',  ( 12.76143908531000193, 9.974460201879001175, 1.751222586102000101 ) ) ;
#13973 = ORIENTED_EDGE ( 'NONE', *, *, #12808, .F. ) ;
#13974 = CARTESIAN_POINT ( 'NONE',  ( -8.687268992921000077, 13.47714631021000109, -4.089943008506000233 ) ) ;
#13975 = DIRECTION ( 'NONE',  ( 1.000000000000000000, 0.000000000000000000, 0.000000000000000000 ) ) ;
#13976 = CARTESIAN_POINT ( 'NONE',  ( 4.000000000000000000, 24.80000000000000426, -2.309401076759000304 ) ) ;
#13977 = ORIENTED_EDGE ( 'NONE', *, *, #1276, .F. ) ;
#13978 = EDGE_CURVE ( 'NONE', #21807, #22775, #20016, .T. ) ;
#13979 = CARTESIAN_POINT ( 'NONE',  ( 11.22311500625409941, 11.82633764590034708, 4.516161837427946857 ) ) ;
#13980 = DIRECTION ( 'NONE',  ( 0.000000000000000000, 1.000000000000000000, 0.000000000000000000 ) ) ;
#13981 = DIRECTION ( 'NONE',  ( 0.000000000000000000, 1.000000000000000000, 0.000000000000000000 ) ) ;
#13982 = CARTESIAN_POINT ( 'NONE',  ( 16.27456687147326164, -0.07827200606447888565, -10.36562678650456881 ) ) ;
#13983 = LINE ( 'NONE', #19567, #3302 ) ;
#13984 = B_SPLINE_CURVE_WITH_KNOTS ( 'NONE', 3,
 ( #13853, #8417, #647, #17372, #19060, #8049, #4414, #13728, #11806, #21256 ),
 .UNSPECIFIED., .F., .F.,
 ( 4, 2, 2, 2, 4 ),
 ( 0.000000000000000000, 0.0005867848385660769540, 0.001173569677132153908, 0.001760354515698231296, 0.002347139354264308683 ),
 .UNSPECIFIED. ) ;
#13985 = CARTESIAN_POINT ( 'NONE',  ( -14.43045988485397935, -9.209646829420966796, 9.048410431333177684 ) ) ;
#13986 = CARTESIAN_POINT ( 'NONE',  ( -0.8545932710616224171, 26.39685207198635553, 4.125402498422513276 ) ) ;
#13987 = CARTESIAN_POINT ( 'NONE',  ( -4.038094091498922289, 13.81604646495375555, -4.860948425493686997 ) ) ;
#13988 = FACE_OUTER_BOUND ( 'NONE', #19431, .T. ) ;
#13989 = CARTESIAN_POINT ( 'NONE',  ( -2.157756447954014334, 30.20979554246039456, 0.1029187449844319868 ) ) ;
#13990 = ORIENTED_EDGE ( 'NONE', *, *, #2278, .T. ) ;
#13991 = CARTESIAN_POINT ( 'NONE',  ( 18.60474491173999922, 0.1088057166755999894, 10.28239292309999797 ) ) ;
#13992 = DIRECTION ( 'NONE',  ( -1.000000000000000000, 0.000000000000000000, 0.000000000000000000 ) ) ;
#13993 = DIRECTION ( 'NONE',  ( 1.000000000000000000, 0.000000000000000000, 0.000000000000000000 ) ) ;
#13994 = ADVANCED_FACE ( 'NONE', ( #458 ), #11270, .F. ) ;
#13995 = CARTESIAN_POINT ( 'NONE',  ( -20.21585241526053522, 10.35035534361658272, -1.764829101647155563 ) ) ;
#13996 = CARTESIAN_POINT ( 'NONE',  ( -24.47970833437434024, -11.33727345183922708, -5.363206565890020094 ) ) ;
#13997 = EDGE_CURVE ( 'NONE', #8124, #1589, #6474, .T. ) ;
#13998 = DIRECTION ( 'NONE',  ( 0.000000000000000000, 1.000000000000000000, 0.000000000000000000 ) ) ;
#13999 = EDGE_LOOP ( 'NONE', ( #16995, #5946, #2003, #20693 ) ) ;
#14000 = FACE_OUTER_BOUND ( 'NONE', #18087, .T. ) ;
#14001 = CIRCLE ( 'NONE', #7806, 10.30000000000000426 ) ;
#14002 = DIRECTION ( 'NONE',  ( 1.000000000000000000, 0.000000000000000000, 0.000000000000000000 ) ) ;
#14003 = CARTESIAN_POINT ( 'NONE',  ( 2.141488944079684931, 27.19972511225902423, 0.5077517406370575248 ) ) ;
#14004 = CARTESIAN_POINT ( 'NONE',  ( 0.000000000000000000, 0.000000000000000000, 0.000000000000000000 ) ) ;
#14005 = CARTESIAN_POINT ( 'NONE',  ( 30.87226923053214378, 37.01856778792605240, 2.673746900119610359 ) ) ;
#14006 = B_SPLINE_SURFACE_WITH_KNOTS ( 'NONE', 3, 3, ( 
 ( #21394, #18281, #20215, #12593 ),
 ( #19979, #12710, #3621, #12929 ),
 ( #18388, #21796, #22030, #5211 ),
 ( #1680, #10895, #8848, #9070 ) ),
 .UNSPECIFIED., .F., .F., .F.,
 ( 4, 4 ),
 ( 4, 4 ),
 ( 0.9881930060304000563, 1.000231509685999942 ),
 ( 0.9965732490345999839, 1.000616174089999921 ),
 .UNSPECIFIED. ) ;
#14007 = ORIENTED_EDGE ( 'NONE', *, *, #23501, .T. ) ;
#14008 = EDGE_CURVE ( 'NONE', #11502, #23288, #19646, .T. ) ;
#14009 = CARTESIAN_POINT ( 'NONE',  ( -1.420784056250328886, 26.52499303979539391, 2.114791243013953270 ) ) ;
#14010 = EDGE_CURVE ( 'NONE', #15589, #889, #15352, .T. ) ;
#14011 = AXIS2_PLACEMENT_3D ( 'NONE', #7751, #20827, #5923 ) ;
#14012 = CARTESIAN_POINT ( 'NONE',  ( -12.53497940801999988, 6.430159825535999296, -13.55186498671000095 ) ) ;
#14013 = CARTESIAN_POINT ( 'NONE',  ( -19.72309750885000312, -4.915363752585999890, 9.961952662738001507 ) ) ;
#14014 = CARTESIAN_POINT ( 'NONE',  ( -13.59789000363999989, 6.208834040094999729, -8.775712258748999517 ) ) ;
#14015 = DIRECTION ( 'NONE',  ( 1.000000000000000000, 0.000000000000000000, 0.000000000000000000 ) ) ;
#14016 = CARTESIAN_POINT ( 'NONE',  ( 13.63624951745999958, 6.911022695730999921, -6.778078827992000122 ) ) ;
#14017 = CARTESIAN_POINT ( 'NONE',  ( 2.184057253797768272, 28.22147922721521240, -0.2997864855702207509 ) ) ;
#14018 = CARTESIAN_POINT ( 'NONE',  ( -14.25394832655999977, 13.93375672974000068, 0.7219259138221999494 ) ) ;
#14019 = CARTESIAN_POINT ( 'NONE',  ( 24.37173283531060619, -9.297778257491829734, 8.895775660514537719 ) ) ;
#14020 = ORIENTED_EDGE ( 'NONE', *, *, #820, .T. ) ;
#14021 = B_SPLINE_CURVE_WITH_KNOTS ( 'NONE', 3,
 ( #3485, #18251, #18360, #1772, #16536, #7336, #18479, #14717, #22113, #5521, #1892, #7446, #22220, #20419, #10631, #22073, #23402, #6947, #21955, #18325, #19794, #16008, #3326, #12862, #3205, #14681, #14212, #3664, #23655, #6820, #10830, #7170, #10939, #1730, #21841, #16263, #18216, #10587, #1503, #17975, #10704, #1376 ),
 .UNSPECIFIED., .F., .F.,
 ( 4, 2, 1, 2, 2, 2, 1, 2, 2, 2, 2, 2, 2, 2, 2, 1, 2, 2, 2, 1, 2, 2, 4 ),
 ( 0.000000000000000000, 0.06249999999999979183, 0.09374999999999969469, 0.1093749999999996392, 0.1249999999999995837, 0.1874999999999995282, 0.2187499999999993616, 0.2343749999999991673, 0.2499999999999989730, 0.3124999999999987788, 0.3749999999999986677, 0.4999999999999984457, 0.5624999999999983347, 0.6249999999999982236, 0.6874999999999981126, 0.7187499999999982236, 0.7343749999999983347, 0.7499999999999983347, 0.8124999999999988898, 0.8437499999999992228, 0.8593749999999993339, 0.8749999999999995559, 1.000000000000000000 ),
 .UNSPECIFIED. ) ;
#14022 = CARTESIAN_POINT ( 'NONE',  ( -2.122180917233752240, 13.91146394560632515, 5.745605564203374982 ) ) ;
#14023 = CARTESIAN_POINT ( 'NONE',  ( 2.070238309910999774, 25.71619850837999977, 0.4658180156273000194 ) ) ;
#14024 = VECTOR ( 'NONE', #2205, 1000.000000000000000 ) ;
#14025 = CARTESIAN_POINT ( 'NONE',  ( -19.24432910583999856, 9.165129126472001175, 0.000000000000000000 ) ) ;
#14026 = CARTESIAN_POINT ( 'NONE',  ( -14.34305601391669427, 6.095070058083463138, -6.708088486029590847 ) ) ;
#14027 = CARTESIAN_POINT ( 'NONE',  ( -1.279883260171999826, 28.48437716036000111, -2.088559871480999419 ) ) ;
#14028 = DIRECTION ( 'NONE',  ( 1.000000000000000000, 0.000000000000000000, 0.000000000000000000 ) ) ;
#14029 = CARTESIAN_POINT ( 'NONE',  ( -4.758298526560081676, 12.41512346299555425, 0.9316463370115228848 ) ) ;
#14030 = EDGE_LOOP ( 'NONE', ( #9836, #14587, #9277, #17240 ) ) ;
#14031 = CARTESIAN_POINT ( 'NONE',  ( -5.194121241778000275, 1.198997689148931003E-14, -12.44999999999999929 ) ) ;
#14032 = CARTESIAN_POINT ( 'NONE',  ( 3.890492083747782104, 12.11396562357843720, -2.873055849959892605 ) ) ;
#14033 = CARTESIAN_POINT ( 'NONE',  ( 66.60588651278291650, 37.01856778792605240, 1.000000000000000000 ) ) ;
#14034 = B_SPLINE_CURVE_WITH_KNOTS ( 'NONE', 3,
 ( #4940, #21766, #18450, #18017, #3129, #4816, #1418, #6623, #8816, #8688, #16177, #21526, #23579, #19468, #12203, #16053, #3002, #23446, #17778, #23207, #6984, #14373, #5179, #12561, #3676, #12086, #10260, #17649 ),
 .UNSPECIFIED., .F., .F.,
 ( 4, 2, 2, 1, 1, 2, 2, 2, 1, 1, 2, 2, 2, 2, 2, 4 ),
 ( 0.000000000000000000, 0.1250000000000167089, 0.1875000000000248412, 0.2187500000000285327, 0.2343750000000297540, 0.2421875000000298650, 0.2500000000000299760, 0.3750000000000260347, 0.4375000000000237588, 0.4687500000000231482, 0.4843750000000227596, 0.5000000000000224265, 0.6250000000000169864, 0.6875000000000139888, 0.7500000000000108802, 1.000000000000000000 ),
 .UNSPECIFIED. ) ;
#14035 = CARTESIAN_POINT ( 'NONE',  ( 11.71313497180072183, -3.220258825039508110, -8.401516397519381840 ) ) ;
#14036 = CARTESIAN_POINT ( 'NONE',  ( 0.000000000000000000, 24.50000000000000000, 0.000000000000000000 ) ) ;
#14037 = CARTESIAN_POINT ( 'NONE',  ( -10.29430721169000051, -2.366881450064000081, 15.38787860124999973 ) ) ;
#14038 = CARTESIAN_POINT ( 'NONE',  ( 11.47028936713000036, -8.379193606113998882, -3.189305674207999708 ) ) ;
#14039 = VECTOR ( 'NONE', #19526, 1000.000000000000000 ) ;
#14040 = CARTESIAN_POINT ( 'NONE',  ( 15.25781392131000125, -9.389200645904999476, -2.369324833533999808 ) ) ;
#14041 = LINE ( 'NONE', #23351, #3951 ) ;
#14042 = ORIENTED_EDGE ( 'NONE', *, *, #275, .F. ) ;
#14043 = CARTESIAN_POINT ( 'NONE',  ( -2.500000000000000444, 28.78333333333333144, -0.3272492347489320275 ) ) ;
#14044 = CARTESIAN_POINT ( 'NONE',  ( -0.4458865764599000414, 29.37709983102000066, -2.493253997570000102 ) ) ;
#14045 = CARTESIAN_POINT ( 'NONE',  ( -15.61632910584000022, 9.072027496059000384, 0.000000000000000000 ) ) ;
#14046 = CARTESIAN_POINT ( 'NONE',  ( 24.50000000000000000, 0.000000000000000000, 0.000000000000000000 ) ) ;
#14047 = VERTEX_POINT ( 'NONE', #5806 ) ;
#14048 = FACE_OUTER_BOUND ( 'NONE', #15320, .T. ) ;
#14049 = CARTESIAN_POINT ( 'NONE',  ( -3.000000000000000000, 17.00000000000000000, 0.000000000000000000 ) ) ;
#14050 = DIRECTION ( 'NONE',  ( 0.000000000000000000, 0.9780930753991020632, 0.2081680471550005351 ) ) ;
#14051 = CARTESIAN_POINT ( 'NONE',  ( 0.000000000000000000, 24.49999999999999645, 0.000000000000000000 ) ) ;
#14052 = CARTESIAN_POINT ( 'NONE',  ( 16.20416496014759034, 4.371488613225747777, -9.447241867773790602 ) ) ;
#14053 = CARTESIAN_POINT ( 'NONE',  ( -3.850316308734367254, 14.01983185593565651, 4.848505112072696299 ) ) ;
#14054 = FACE_OUTER_BOUND ( 'NONE', #9200, .T. ) ;
#14055 = CARTESIAN_POINT ( 'NONE',  ( -24.37124162823073448, -9.546779961752369204, 8.464497487801450504 ) ) ;
#14056 = ORIENTED_EDGE ( 'NONE', *, *, #12669, .T. ) ;
#14057 = CARTESIAN_POINT ( 'NONE',  ( 2.424643331163519964E-11, 24.52694564545263844, -2.373054354547839306 ) ) ;
#14058 = DIRECTION ( 'NONE',  ( 0.000000000000000000, 1.000000000000000000, 0.000000000000000000 ) ) ;
#14059 = ORIENTED_EDGE ( 'NONE', *, *, #3593, .F. ) ;
#14060 = CARTESIAN_POINT ( 'NONE',  ( -1.662092656101999966, 23.94309775297999821, -2.174644641551999769 ) ) ;
#14061 = DIRECTION ( 'NONE',  ( -1.000000000000000000, 0.000000000000000000, 0.000000000000000000 ) ) ;
#14062 = CARTESIAN_POINT ( 'NONE',  ( 2.058318499670220625, 12.94702448370908776, 6.380432469888065228 ) ) ;
#14063 = CARTESIAN_POINT ( 'NONE',  ( 6.202279051248352992, 13.86702088811886036, -0.9424181477496827997 ) ) ;
#14064 = CARTESIAN_POINT ( 'NONE',  ( -5.978103862651994227, 15.83376621642000792, -0.9317320578097998407 ) ) ;
#14065 = CIRCLE ( 'NONE', #22556, 4.000000000000000000 ) ;
#14066 = B_SPLINE_CURVE_WITH_KNOTS ( 'NONE', 3,
 ( #8959, #11247, #12591, #2032, #22028, #5208, #9185, #5548, #16679, #7472 ),
 .UNSPECIFIED., .F., .F.,
 ( 4, 2, 2, 2, 4 ),
 ( 0.000000000000000000, 0.1250000000000000000, 0.2500000000000000000, 0.5000000000000001110, 1.000000000000000000 ),
 .UNSPECIFIED. ) ;
#14067 = EDGE_LOOP ( 'NONE', ( #6129, #18059, #13571 ) ) ;
#14068 = FACE_OUTER_BOUND ( 'NONE', #9464, .T. ) ;
#14069 = CARTESIAN_POINT ( 'NONE',  ( 0.000000000000000000, 18.89999999999999858, 0.000000000000000000 ) ) ;
#14070 = DIRECTION ( 'NONE',  ( 0.000000000000000000, -1.000000000000000000, 0.000000000000000000 ) ) ;
#14071 = ORIENTED_EDGE ( 'NONE', *, *, #12542, .T. ) ;
#14072 = CARTESIAN_POINT ( 'NONE',  ( -19.16110032286999854, -4.005958525575000095, 9.301206193175998393 ) ) ;
#14073 = CARTESIAN_POINT ( 'NONE',  ( 21.02020833333332561, 9.210701687524210257, -1.205804979152639733 ) ) ;
#14074 = CARTESIAN_POINT ( 'NONE',  ( 15.06774083095429440, 8.954513157289483161, 5.161873896049346655 ) ) ;
#14075 = FACE_OUTER_BOUND ( 'NONE', #16522, .T. ) ;
#14076 = ADVANCED_FACE ( 'NONE', ( #3991 ), #12007, .F. ) ;
#14077 = CARTESIAN_POINT ( 'NONE',  ( -12.25000000000000000, -13.93375672974000068, 0.000000000000000000 ) ) ;
#14078 = CARTESIAN_POINT ( 'NONE',  ( -22.52702113186910893, -5.641063948273841611, 7.354633707470615178 ) ) ;
#14079 = CARTESIAN_POINT ( 'NONE',  ( 4.628885738981002085, 12.57105835719000275, -1.073190880219000221 ) ) ;
#14080 = EDGE_LOOP ( 'NONE', ( #9383, #20948, #4481, #3612 ) ) ;
#14081 = CARTESIAN_POINT ( 'NONE',  ( -15.47399649439000058, -8.448196802485998802, -7.562854223976000156 ) ) ;
#14082 = CARTESIAN_POINT ( 'NONE',  ( -1.524685720705258207, 29.50411617716720514, 1.529777632466581050 ) ) ;
#14083 = VERTEX_POINT ( 'NONE', #14033 ) ;
#14084 = CARTESIAN_POINT ( 'NONE',  ( 1.999167105995449889, 29.28333333333333499, -1.536366799937288086 ) ) ;
#14085 = CARTESIAN_POINT ( 'NONE',  ( -15.67845997203782105, -8.965097180577222602, -5.248789696445946618 ) ) ;
#14086 = ORIENTED_EDGE ( 'NONE', *, *, #1963, .F. ) ;
#14087 = CARTESIAN_POINT ( 'NONE',  ( 5.922047466466997534, 13.79009778142999920, -2.080318915485001252 ) ) ;
#14088 = EDGE_CURVE ( 'NONE', #7062, #8639, #14210, .T. ) ;
#14089 = CARTESIAN_POINT ( 'NONE',  ( 12.00000000000000000, -1.672630921217244993, -8.822341735481002090 ) ) ;
#14090 = CARTESIAN_POINT ( 'NONE',  ( 18.99010413682999854, -5.601003484193999959, 8.806426514188000709 ) ) ;
#14091 = CARTESIAN_POINT ( 'NONE',  ( -1.938452583514000072, 27.67006359724000220, 1.528152797339000113 ) ) ;
#14092 = CARTESIAN_POINT ( 'NONE',  ( 16.05206408531000051, 5.563243567929000655, -8.565419716155998842 ) ) ;
#14093 = ORIENTED_EDGE ( 'NONE', *, *, #1695, .T. ) ;
#14094 = CARTESIAN_POINT ( 'NONE',  ( -8.992736492921000746, -0.04910128871962000235, -14.51750318222000047 ) ) ;
#14095 = DIRECTION ( 'NONE',  ( -1.000000000000000000, 0.000000000000000000, 0.000000000000000000 ) ) ;
#14096 = CARTESIAN_POINT ( 'NONE',  ( -8.000000000000000000, 1.322618543078999814E-14, 0.000000000000000000 ) ) ;
#14097 = ORIENTED_EDGE ( 'NONE', *, *, #1541, .F. ) ;
#14098 = CARTESIAN_POINT ( 'NONE',  ( -24.00109171669999952, -9.333314996567999344, -0.6894523598369000084 ) ) ;
#14099 = CARTESIAN_POINT ( 'NONE',  ( 11.29022434644395467, 12.01543594605562504, 4.188602139394846269 ) ) ;
#14100 = CONICAL_SURFACE ( 'NONE', #21044, 3.049999825846000157, 0.7853981633972997312 ) ;
#14101 = DIRECTION ( 'NONE',  ( -1.000000000000000000, 0.000000000000000000, 0.000000000000000000 ) ) ;
#14102 = CARTESIAN_POINT ( 'NONE',  ( -6.250000000003001155, 15.09565008225999883, -3.212814891752000079 ) ) ;
#14103 = CARTESIAN_POINT ( 'NONE',  ( 17.52130432638741198, -9.628271833752394926, 4.056250497054570303 ) ) ;
#14104 = CARTESIAN_POINT ( 'NONE',  ( -18.52628743917332699, -7.314404681686845322, 5.620986415498060218 ) ) ;
#14105 = ADVANCED_FACE ( 'NONE', ( #13908 ), #17292, .T. ) ;
#14106 = DIRECTION ( 'NONE',  ( -1.000000000000000000, 0.000000000000000000, 0.000000000000000000 ) ) ;
#14107 = AXIS2_PLACEMENT_3D ( 'NONE', #2971, #17380, #1156 ) ;
#14108 = CARTESIAN_POINT ( 'NONE',  ( 0.000000000000000000, -1.550000000000000044, 0.000000000000000000 ) ) ;
#14109 = CARTESIAN_POINT ( 'NONE',  ( 2.267779804951839839, 26.36777980495183726, 5.387954023152814032E-08 ) ) ;
#14110 = CARTESIAN_POINT ( 'NONE',  ( -1.597028793744863506, 30.29838184876847151, 1.461961021377746972 ) ) ;
#14111 = EDGE_LOOP ( 'NONE', ( #4650, #14389, #11111, #22053, #2914 ) ) ;
#14112 = CARTESIAN_POINT ( 'NONE',  ( -0.6558363950912000639, 25.57813856944000008, 2.241719613464999927 ) ) ;
#14113 = CARTESIAN_POINT ( 'NONE',  ( 20.47283726948000293, -1.948504986539999928, 10.68962299628999979 ) ) ;
#14114 = CARTESIAN_POINT ( 'NONE',  ( 22.85285366138076313, -7.483697671837180820, 7.491427571326791046 ) ) ;
#14115 = CARTESIAN_POINT ( 'NONE',  ( 0.000000000000000000, 15.05000017415440006, -3.049999825846000157 ) ) ;
#14116 = ORIENTED_EDGE ( 'NONE', *, *, #5008, .F. ) ;
#14117 = DIRECTION ( 'NONE',  ( 0.7071067811865474617, 0.7071067811865474617, 0.000000000000000000 ) ) ;
#14118 = CARTESIAN_POINT ( 'NONE',  ( 4.852182833551873742, 14.56344984251652619, 3.781189165742629754 ) ) ;
#14119 = EDGE_CURVE ( 'NONE', #19360, #22068, #19240, .T. ) ;
#14120 = CARTESIAN_POINT ( 'NONE',  ( 4.896390829840998826, 12.43229641542999886, -0.5248650586911998150 ) ) ;
#14121 = ORIENTED_EDGE ( 'NONE', *, *, #19488, .F. ) ;
#14122 = CARTESIAN_POINT ( 'NONE',  ( -15.03279338263535436, 5.021830743698944666, -9.069083216823218052 ) ) ;
#14123 = CARTESIAN_POINT ( 'NONE',  ( 2.500000000000000000, 18.50000000000000000, 0.000000000000000000 ) ) ;
#14124 = ORIENTED_EDGE ( 'NONE', *, *, #23419, .T. ) ;
#14125 = CIRCLE ( 'NONE', #564, 12.50000000000000000 ) ;
#14126 = CARTESIAN_POINT ( 'NONE',  ( 2.049260319077078840, 26.47238454635797922, -0.7136609902301204178 ) ) ;
#14127 = CARTESIAN_POINT ( 'NONE',  ( 0.000000000000000000, 0.000000000000000000, 0.000000000000000000 ) ) ;
#14128 = ADVANCED_FACE ( 'NONE', ( #8589 ), #16128, .T. ) ;
#14129 = CARTESIAN_POINT ( 'NONE',  ( -1.989999999999999991, 0.000000000000000000, 0.000000000000000000 ) ) ;
#14130 = EDGE_LOOP ( 'NONE', ( #8555, #23761, #20555, #4218 ) ) ;
#14131 = CARTESIAN_POINT ( 'NONE',  ( 11.74999999482999868, 0.000000000000000000, -7.249999994832990069 ) ) ;
#14132 = CARTESIAN_POINT ( 'NONE',  ( -12.21107666535000114, 9.613013645102999050, -12.04164784824000023 ) ) ;
#14133 = CARTESIAN_POINT ( 'NONE',  ( -21.16837767356999578, -10.99666358480999939, -1.827877429396000064 ) ) ;
#14134 = EDGE_CURVE ( 'NONE', #13647, #3316, #12224, .T. ) ;
#14135 = CARTESIAN_POINT ( 'NONE',  ( -16.50776531261999835, -8.025729601713999628, 6.450400044432999636 ) ) ;
#14136 = CARTESIAN_POINT ( 'NONE',  ( -5.988267586462001191, 16.12301021452999805, 0.9718889544497001376 ) ) ;
#14137 = ADVANCED_FACE ( 'NONE', ( #23345 ), #2899, .T. ) ;
#14138 = CARTESIAN_POINT ( 'NONE',  ( 16.20869494526000310, -9.667040997353000265, 3.533098828328999907 ) ) ;
#14139 = DIRECTION ( 'NONE',  ( 0.000000000000000000, -1.000000000000000000, 0.000000000000000000 ) ) ;
#14140 = DIRECTION ( 'NONE',  ( 0.000000000000000000, 0.000000000000000000, 1.000000000000000000 ) ) ;
#14141 = CARTESIAN_POINT ( 'NONE',  ( 15.08691666666666187, -2.371145242616797599, -8.822626156915163165 ) ) ;
#14142 = ORIENTED_EDGE ( 'NONE', *, *, #15163, .F. ) ;
#14143 = CARTESIAN_POINT ( 'NONE',  ( 23.56203090460532934, 1.574364913339408867, 9.158349804732198507 ) ) ;
#14144 = CARTESIAN_POINT ( 'NONE',  ( -2.218848708602919384, 13.93185214957625817, 5.709114769721670868 ) ) ;
#14145 = CARTESIAN_POINT ( 'NONE',  ( -1.780325977227999790, 27.82869850838000048, 1.403495832404999977 ) ) ;
#14146 = CIRCLE ( 'NONE', #6001, 3.100000000000000089 ) ;
#14147 = CARTESIAN_POINT ( 'NONE',  ( 23.41677564524290744, 35.51856778792605240, 6.000000000000000000 ) ) ;
#14148 = CARTESIAN_POINT ( 'NONE',  ( -22.75062164853999747, 0.1503650050700000018, -11.12440192913999937 ) ) ;
#14149 = ADVANCED_FACE ( 'NONE', ( #13544 ), #11510, .F. ) ;
#14150 = EDGE_CURVE ( 'NONE', #4798, #2581, #19849, .T. ) ;
#14151 = CARTESIAN_POINT ( 'NONE',  ( -4.511714276356390663, 12.32404474554762785, 1.769770020287825263 ) ) ;
#14152 = EDGE_LOOP ( 'NONE', ( #16320, #10991, #8496, #10811 ) ) ;
#14153 = CYLINDRICAL_SURFACE ( 'NONE', #19200, 7.000000000000000000 ) ;
#14154 = CARTESIAN_POINT ( 'NONE',  ( -24.49594166687865027, -0.5121745395713884763, -12.49996680834449947 ) ) ;
#14155 = CARTESIAN_POINT ( 'NONE',  ( 24.06454052246407826, -3.752188697602235390, -8.644687579573476555 ) ) ;
#14156 = CARTESIAN_POINT ( 'NONE',  ( -21.16580420454666367, 7.368390746024480187, 5.662792393064417062 ) ) ;
#14157 = VECTOR ( 'NONE', #18336, 1000.000000000000000 ) ;
#14158 = CARTESIAN_POINT ( 'NONE',  ( 2.184465970885655306, 24.33333333333333570, 1.259047450927230027 ) ) ;
#14159 = CARTESIAN_POINT ( 'NONE',  ( -17.91156067002999919, -1.604197317876000062, 11.29338059605000133 ) ) ;
#14160 = VECTOR ( 'NONE', #18289, 1000.000000000000000 ) ;
#14161 = CARTESIAN_POINT ( 'NONE',  ( 14.49000142131000146, 7.205444258087999820, 6.439089808501999634 ) ) ;
#14162 = CARTESIAN_POINT ( 'NONE',  ( 24.28255857084583624, 4.111234970449187287, 12.50000000000000533 ) ) ;
#14163 = ORIENTED_EDGE ( 'NONE', *, *, #18157, .T. ) ;
#14164 = CARTESIAN_POINT ( 'NONE',  ( 5.302311171175275284, 13.76370502379775118, 4.348021967961785528 ) ) ;
#14165 = CARTESIAN_POINT ( 'NONE',  ( -0.3904964477860000116, 29.04133632509000051, 2.613711361504000408 ) ) ;
#14166 = CARTESIAN_POINT ( 'NONE',  ( -14.74712077250667086, -9.049721897106270063, 1.184478878552067682 ) ) ;
#14167 = CARTESIAN_POINT ( 'NONE',  ( 4.071856426817071828, 14.48689095887983846, -4.575612886981444305 ) ) ;
#14168 = ORIENTED_EDGE ( 'NONE', *, *, #3038, .F. ) ;
#14169 = CARTESIAN_POINT ( 'NONE',  ( -1.236362846991004183, 26.50000008335574719, -2.171602059085420589 ) ) ;
#14170 = FACE_OUTER_BOUND ( 'NONE', #22405, .T. ) ;
#14171 = DIRECTION ( 'NONE',  ( 1.000000000000000000, 0.000000000000000000, 0.000000000000000000 ) ) ;
#14172 = CARTESIAN_POINT ( 'NONE',  ( -5.695156607585949438, 16.22280606751403198, 2.279197634692520680 ) ) ;
#14173 = CARTESIAN_POINT ( 'NONE',  ( 16.12053336643119295, 1.488762681687257672, -10.30218658287923716 ) ) ;
#14174 = CARTESIAN_POINT ( 'NONE',  ( -4.066544995498063031, 13.78971146288197325, 4.867452680521627606 ) ) ;
#14175 = CARTESIAN_POINT ( 'NONE',  ( 4.942518863364997017, 12.51350827579999958, 0.2556867146312000183 ) ) ;
#14176 = CARTESIAN_POINT ( 'NONE',  ( -23.50032910583999879, 1.512442827330999945E-14, 0.000000000000000000 ) ) ;
#14177 = EDGE_LOOP ( 'NONE', ( #13923, #14925, #10242, #22292 ) ) ;
#14178 = EDGE_CURVE ( 'NONE', #7012, #1, #6397, .T. ) ;
#14179 = FACE_OUTER_BOUND ( 'NONE', #2592, .T. ) ;
#14180 = CIRCLE ( 'NONE', #2183, 9.274346474608000435 ) ;
#14181 = CARTESIAN_POINT ( 'NONE',  ( 1.699999994525651204, 12.91209873359414217, 1.053565370275990620 ) ) ;
#14182 = CIRCLE ( 'NONE', #13006, 3.000000000000000000 ) ;
#14183 = VERTEX_POINT ( 'NONE', #8709 ) ;
#14184 = CARTESIAN_POINT ( 'NONE',  ( 2.247878665003999910, 25.86878373060999792, -0.3542756539240000668 ) ) ;
#14185 = CARTESIAN_POINT ( 'NONE',  ( 6.124486376501002916, 14.49660437619998810, 0.3689214650952001295 ) ) ;
#14186 = CARTESIAN_POINT ( 'NONE',  ( -0.4921054408743313346, 12.81188039431768644, 6.647493645939474227 ) ) ;
#14187 = CARTESIAN_POINT ( 'NONE',  ( 4.750000000000000000, 16.89999999999999858, 0.000000000000000000 ) ) ;
#14188 = CARTESIAN_POINT ( 'NONE',  ( -6.012535197899005368, 16.49418337425001013, -1.225408514526999282 ) ) ;
#14189 = CARTESIAN_POINT ( 'NONE',  ( 0.000000000000000000, 15.05000017415440006, 0.000000000000000000 ) ) ;
#14190 = AXIS2_PLACEMENT_3D ( 'NONE', #19333, #12187, #8308 ) ;
#14191 = VERTEX_POINT ( 'NONE', #23819 ) ;
#14192 = CARTESIAN_POINT ( 'NONE',  ( -12.24999999999999822, 13.59206128970241778, -6.344557540553090291 ) ) ;
#14193 = DIRECTION ( 'NONE',  ( 0.000000000000000000, 1.000000000000000000, 0.000000000000000000 ) ) ;
#14194 = DIRECTION ( 'NONE',  ( 0.000000000000000000, -1.000000000000000000, 0.000000000000000000 ) ) ;
#14195 = ORIENTED_EDGE ( 'NONE', *, *, #13699, .T. ) ;
#14196 = CARTESIAN_POINT ( 'NONE',  ( -23.24757862902999861, -5.490534083007999833, 9.858273392202999474 ) ) ;
#14197 = CIRCLE ( 'NONE', #13397, 3.000000000000000000 ) ;
#14198 = LINE ( 'NONE', #21595, #20743 ) ;
#14199 = CARTESIAN_POINT ( 'NONE',  ( 14.88837544317048511, 10.27747569187551235, -1.051874237603601436 ) ) ;
#14200 = CARTESIAN_POINT ( 'NONE',  ( 4.000000000000000000, 24.80000000000000426, 2.309401076759000304 ) ) ;
#14201 = DIRECTION ( 'NONE',  ( 0.000000000000000000, 1.000000000000000000, 0.000000000000000000 ) ) ;
#14202 = FACE_OUTER_BOUND ( 'NONE', #18966, .T. ) ;
#14203 = CARTESIAN_POINT ( 'NONE',  ( -4.725411482781997741, 12.53696406558999143, -0.01086751525878999931 ) ) ;
#14204 = EDGE_LOOP ( 'NONE', ( #12021, #6091, #13961, #17816, #2456, #12041 ) ) ;
#14205 = CARTESIAN_POINT ( 'NONE',  ( -10.25814758309999952, -7.142857142857000241, 0.000000000000000000 ) ) ;
#14206 = CARTESIAN_POINT ( 'NONE',  ( -1.633105399745039321, 29.31302638303034058, -1.413471024401691256 ) ) ;
#14207 = VERTEX_POINT ( 'NONE', #1788 ) ;
#14208 = CARTESIAN_POINT ( 'NONE',  ( 2.184465970885645092, 29.26666666666667993, -1.259047450927249123 ) ) ;
#14209 = CARTESIAN_POINT ( 'NONE',  ( -14.57877136579895705, 3.775861415940093835, 9.652007294606121945 ) ) ;
#14210 = CIRCLE ( 'NONE', #7243, 12.44999999999999574 ) ;
#14211 = VERTEX_POINT ( 'NONE', #16201 ) ;
#14212 = CARTESIAN_POINT ( 'NONE',  ( 11.22311500625338354, -11.82633764589515302, -4.516161837439471860 ) ) ;
#14213 = AXIS2_PLACEMENT_3D ( 'NONE', #11361, #7836, #5892 ) ;
#14214 = CARTESIAN_POINT ( 'NONE',  ( 12.00000000000000000, 0.7795197778698420565, -8.945416492546511833 ) ) ;
#14215 = CONICAL_SURFACE ( 'NONE', #6065, 9.630770167580999797, 0.9419447502231289571 ) ;
#14216 = DIRECTION ( 'NONE',  ( -1.000000000000000000, 0.000000000000000000, 0.000000000000000000 ) ) ;
#14217 = ADVANCED_FACE ( 'NONE', ( #7229 ), #16555, .T. ) ;
#14218 = CARTESIAN_POINT ( 'NONE',  ( -2.456483904114000083, 27.57256359724000205, -0.2419425476017999788 ) ) ;
#14219 = CARTESIAN_POINT ( 'NONE',  ( 13.74862658530999937, -9.135377135809001459, -4.430325866828999537 ) ) ;
#14220 = VERTEX_POINT ( 'NONE', #21672 ) ;
#14221 = DIRECTION ( 'NONE',  ( 0.000000000000000000, 1.000000000000000000, 0.000000000000000000 ) ) ;
#14222 = B_SPLINE_CURVE_WITH_KNOTS ( 'NONE', 3,
 ( #12813, #20090, #20203, #19740, #19967, #1320, #21899, #14505 ),
 .UNSPECIFIED., .F., .F.,
 ( 4, 2, 2, 4 ),
 ( 0.000000000000000000, 0.2500000000000000000, 0.5000000000000000000, 1.000000000000000000 ),
 .UNSPECIFIED. ) ;
#14223 = PLANE ( 'NONE',  #17111 ) ;
#14224 = ORIENTED_EDGE ( 'NONE', *, *, #21707, .T. ) ;
#14225 = CARTESIAN_POINT ( 'NONE',  ( 11.22285964980139283, 9.825076113690533575, 7.982449282869310103 ) ) ;
#14226 = CARTESIAN_POINT ( 'NONE',  ( 22.44108499922769795, -0.4819289312304581574, 10.56690249824243466 ) ) ;
#14227 = CARTESIAN_POINT ( 'NONE',  ( 17.03668726726226268, 5.064517129654977801, 9.097274685846976183 ) ) ;
#14228 = AXIS2_PLACEMENT_3D ( 'NONE', #14036, #11986, #6399 ) ;
#14229 = CARTESIAN_POINT ( 'NONE',  ( -18.33732910583999853, -9.141853718868999223, 0.000000000000000000 ) ) ;
#14230 = EDGE_CURVE ( 'NONE', #2430, #20052, #14222, .T. ) ;
#14231 = CARTESIAN_POINT ( 'NONE',  ( 0.2323400247800999907, 29.20173034859999817, -2.331423980350999958 ) ) ;
#14232 = CARTESIAN_POINT ( 'NONE',  ( -4.475682853278175166, 13.51377492745002229, -5.070986449459744527 ) ) ;
#14233 = CARTESIAN_POINT ( 'NONE',  ( -2.124536007966489670, 30.18061194770063338, -0.3918411660969223775 ) ) ;
#14234 = VERTEX_POINT ( 'NONE', #14277 ) ;
#14235 = CARTESIAN_POINT ( 'NONE',  ( 2.333600034839999893, 25.01975644544999966, -0.09865051850806999534 ) ) ;
#14236 = CARTESIAN_POINT ( 'NONE',  ( 23.61741393687999846, 8.209328251910999796, -8.036582473515998970 ) ) ;
#14237 = CARTESIAN_POINT ( 'NONE',  ( 3.999987874060709991, 28.10222989788994497, -1.328900689436832261 ) ) ;
#14238 = CARTESIAN_POINT ( 'NONE',  ( -6.000000000000000000, 28.00000000000000000, -6.000000000000000000 ) ) ;
#14239 = ORIENTED_EDGE ( 'NONE', *, *, #14088, .F. ) ;
#14240 = DIRECTION ( 'NONE',  ( 0.000000000000000000, 1.000000000000000000, 0.000000000000000000 ) ) ;
#14241 = CARTESIAN_POINT ( 'NONE',  ( 4.871525856247341579, 14.47411258586163285, 3.795094578399595520 ) ) ;
#14242 = AXIS2_PLACEMENT_3D ( 'NONE', #5910, #22261, #20694 ) ;
#14243 = CARTESIAN_POINT ( 'NONE',  ( 0.3813121960981003533, 11.52964601297000335, -4.965239699173999988 ) ) ;
#14244 = EDGE_LOOP ( 'NONE', ( #23705, #3162, #4837 ) ) ;
#14245 = B_SPLINE_CURVE_WITH_KNOTS ( 'NONE', 3,
 ( #16763, #530, #13144, #15184, #15068, #9279, #20299, #22579, #11093, #5756, #7563, #7934, #14943, #22462, #15301, #3945, #4178, #13257, #20650, #1891, #59, #17014, #20537, #7444, #12898, #413, #18710, #5520, #2120, #9509, #11454, #18830, #7812, #13369, #8298, #23183, #2852, #2731, #8549, #21376, #8178, #15427, #17502, #15546, #19322, #12176, #19443, #10233, #10362, #22814, #11936 ),
 .UNSPECIFIED., .F., .F.,
 ( 4, 1, 1, 2, 2, 1, 1, 1, 1, 1, 2, 2, 1, 1, 1, 1, 1, 2, 2, 1, 1, 1, 1, 1, 2, 2, 1, 1, 1, 2, 2, 2, 1, 2, 2, 4 ),
 ( 0.000000000000000000, 0.06250000000000245637, 0.09375000000000369149, 0.1093750000000042744, 0.1250000000000048572, 0.1875000000000070499, 0.2187500000000081324, 0.2343750000000086597, 0.2421875000000089095, 0.2460937500000090206, 0.2480468750000090761, 0.2500000000000091038, 0.3125000000000100475, 0.3437500000000105471, 0.3593750000000108247, 0.3671875000000109912, 0.3710937500000111022, 0.3730468750000111022, 0.3750000000000111022, 0.4375000000000130451, 0.4687500000000140443, 0.4843750000000145439, 0.4921875000000148770, 0.4960937500000149325, 0.4980468750000149880, 0.5000000000000149880, 0.5625000000000126565, 0.5937500000000114353, 0.6093750000000108802, 0.6171875000000106581, 0.6250000000000105471, 0.7500000000000069944, 0.8125000000000053291, 0.8437500000000044409, 0.8750000000000035527, 1.000000000000000000 ),
 .UNSPECIFIED. ) ;
#14246 = EDGE_CURVE ( 'NONE', #23264, #18727, #15652, .T. ) ;
#14247 = CARTESIAN_POINT ( 'NONE',  ( 17.53481375730999758, 8.357543471651000644, -3.927243979254000372 ) ) ;
#14248 = ORIENTED_EDGE ( 'NONE', *, *, #23093, .F. ) ;
#14249 = DIRECTION ( 'NONE',  ( -1.000000000000000000, 0.000000000000000000, 0.000000000000000000 ) ) ;
#14250 = PRESENTATION_LAYER_ASSIGNMENT (  '', '', ( #5735 ) ) ;
#14251 = DIRECTION ( 'NONE',  ( 0.000000000000000000, 0.000000000000000000, 1.000000000000000000 ) ) ;
#14252 = VERTEX_POINT ( 'NONE', #22238 ) ;
#14253 = CARTESIAN_POINT ( 'NONE',  ( -18.79994503103667469, -7.728185936305688841, 5.020550006176206281 ) ) ;
#14254 = CARTESIAN_POINT ( 'NONE',  ( -11.96502059198000012, 13.67685060524999940, -6.159850446377999056 ) ) ;
#14255 = CARTESIAN_POINT ( 'NONE',  ( -21.43755845894000345, -10.49164694751999960, -1.743970444100000128 ) ) ;
#14256 = EDGE_CURVE ( 'NONE', #6193, #8075, #1454, .T. ) ;
#14257 = CARTESIAN_POINT ( 'NONE',  ( -0.3463667137703017040, 24.70780860099542764, 4.418706525546099328 ) ) ;
#14258 = CARTESIAN_POINT ( 'NONE',  ( 24.50000000000000000, -9.344098705406999272, -3.489386534399999906 ) ) ;
#14259 = CARTESIAN_POINT ( 'NONE',  ( 2.125092041327180326, 26.63141011545438985, -0.4551239170173230764 ) ) ;
#14260 = AXIS2_PLACEMENT_3D ( 'NONE', #10042, #12101, #17298 ) ;
#14261 = DIRECTION ( 'NONE',  ( 0.000000000000000000, 0.9512662730843030046, -0.3083706822840010520 ) ) ;
#14262 = CARTESIAN_POINT ( 'NONE',  ( 24.43449445986659896, -9.725059455069036574, 8.155702917191968382 ) ) ;
#14263 = ORIENTED_EDGE ( 'NONE', *, *, #15278, .F. ) ;
#14264 = CARTESIAN_POINT ( 'NONE',  ( -0.3564538054804341494, 26.29977277844468020, -4.413003452969197049 ) ) ;
#14265 = CARTESIAN_POINT ( 'NONE',  ( -12.50000000000000000, 1.557342902441000195E-14, 0.000000000000000000 ) ) ;
#14266 = CARTESIAN_POINT ( 'NONE',  ( 1.107772814030999919, 25.87869850838000119, -1.978081431919000099 ) ) ;
#14267 = EDGE_CURVE ( 'NONE', #3203, #22477, #18551, .T. ) ;
#14268 = CIRCLE ( 'NONE', #20064, 15.43375672974000068 ) ;
#14269 = CARTESIAN_POINT ( 'NONE',  ( 0.5249584007626000304, 28.38687716036000097, -2.392615059649000120 ) ) ;
#14270 = AXIS2_PLACEMENT_3D ( 'NONE', #23457, #1308, #3251 ) ;
#14271 = CIRCLE ( 'NONE', #17771, 4.750000000000000000 ) ;
#14272 = CARTESIAN_POINT ( 'NONE',  ( 0.03709750155276533845, 11.48001782603875576, 4.817879853919041722 ) ) ;
#14273 = VERTEX_POINT ( 'NONE', #22131 ) ;
#14274 = CARTESIAN_POINT ( 'NONE',  ( 6.243179582884000212, 1.148189900220999940E-14, 0.000000000000000000 ) ) ;
#14275 = EDGE_CURVE ( 'NONE', #8479, #1455, #16672, .T. ) ;
#14276 = CARTESIAN_POINT ( 'NONE',  ( 3.408454823722866678, 11.96990078945976954, -3.424875488495797704 ) ) ;
#14277 = CARTESIAN_POINT ( 'NONE',  ( 11.00000000000000000, 7.000000000000000000, 0.000000000000000000 ) ) ;
#14278 = CIRCLE ( 'NONE', #8106, 7.500000000000000000 ) ;
#14279 = CARTESIAN_POINT ( 'NONE',  ( -20.63672087121333476, -7.357712943626705027, 5.654268963819235161 ) ) ;
#14280 = VERTEX_POINT ( 'NONE', #12920 ) ;
#14281 = CARTESIAN_POINT ( 'NONE',  ( -2.434931691670770171, 24.03333333333333499, 0.6543697108982720057 ) ) ;
#14282 = CARTESIAN_POINT ( 'NONE',  ( -13.03643231875999930, 10.05168146521000061, -2.584826834016999531 ) ) ;
#14283 = CARTESIAN_POINT ( 'NONE',  ( 13.83187642131000139, 0.1979999634357000049, -9.644016179210000317 ) ) ;
#14284 = CARTESIAN_POINT ( 'NONE',  ( 18.84514110817610089, 5.243717532068479237, 9.030486612376559918 ) ) ;
#14285 = VECTOR ( 'NONE', #17159, 1000.000000000000114 ) ;
#14286 = ORIENTED_EDGE ( 'NONE', *, *, #14735, .F. ) ;
#14287 = ADVANCED_FACE ( 'NONE', ( #4081 ), #18456, .T. ) ;
#14288 = CARTESIAN_POINT ( 'NONE',  ( 5.239091540984079920, 13.88197682617082762, 4.112037740998657043 ) ) ;
#14289 = CARTESIAN_POINT ( 'NONE',  ( -1.879209721347999906, 30.33054072803999901, 1.397325483377999999 ) ) ;
#14290 = CARTESIAN_POINT ( 'NONE',  ( 0.5271288625574210851, 26.26111511314614688, 2.095841999210956264 ) ) ;
#14291 = CARTESIAN_POINT ( 'NONE',  ( 13.50000000000000000, -9.063837456487554789, 4.006327031784646664 ) ) ;
#14292 = AXIS2_PLACEMENT_3D ( 'NONE', #14831, #22226, #5638 ) ;
#14293 = EDGE_LOOP ( 'NONE', ( #3330, #14346, #19059, #2344 ) ) ;
#14294 = DIRECTION ( 'NONE',  ( 0.000000000000000000, 1.000000000000000000, 0.000000000000000000 ) ) ;
#14295 = FACE_OUTER_BOUND ( 'NONE', #8538, .T. ) ;
#14296 = PLANE ( 'NONE',  #2645 ) ;
#14297 = CARTESIAN_POINT ( 'NONE',  ( -12.50000000000000000, 6.739397414018897692, -5.973639980163532925 ) ) ;
#14298 = CARTESIAN_POINT ( 'NONE',  ( 14.81030506489262777, 9.856952506639157008, 3.248035065178327851 ) ) ;
#14299 = PLANE ( 'NONE',  #16841 ) ;
#14300 = AXIS2_PLACEMENT_3D ( 'NONE', #3812, #3932, #9497 ) ;
#14301 = CARTESIAN_POINT ( 'NONE',  ( -4.861444494134998351, 12.41891182900000601, 0.7440676659160004869 ) ) ;
#14302 = CARTESIAN_POINT ( 'NONE',  ( 20.28412270046332821, -8.031631873314140080, 4.629288412270770259 ) ) ;
#14303 = ORIENTED_EDGE ( 'NONE', *, *, #17844, .F. ) ;
#14304 = DIRECTION ( 'NONE',  ( 1.000000000000000000, 0.000000000000000000, 0.000000000000000000 ) ) ;
#14305 = CARTESIAN_POINT ( 'NONE',  ( -4.000000000000000000, 26.50000000000000355, 0.000000000000000000 ) ) ;
#14306 = EDGE_LOOP ( 'NONE', ( #7367, #21460, #2713 ) ) ;
#14307 = AXIS2_PLACEMENT_3D ( 'NONE', #13326, #7887, #2079 ) ;
#14308 = CARTESIAN_POINT ( 'NONE',  ( 0.4324689435440000063, 24.63980054822999932, -2.702762649533999806 ) ) ;
#14309 = EDGE_CURVE ( 'NONE', #2155, #17483, #3013, .T. ) ;
#14310 = CARTESIAN_POINT ( 'NONE',  ( 6.093726023679999493, 14.50411598793998635, 0.7125610185517002870 ) ) ;
#14311 = CARTESIAN_POINT ( 'NONE',  ( 11.39490977864336330, -2.886098606921414955, -12.49995748308249865 ) ) ;
#14312 = EDGE_CURVE ( 'NONE', #8412, #6193, #7585, .T. ) ;
#14313 = AXIS2_PLACEMENT_3D ( 'NONE', #7148, #9095, #16468 ) ;
#14314 = CARTESIAN_POINT ( 'NONE',  ( 6.235934676345907590, 13.70700678873121880, -1.537716637499378258 ) ) ;
#14315 = FACE_OUTER_BOUND ( 'NONE', #20845, .T. ) ;
#14316 = DIRECTION ( 'NONE',  ( 0.000000000000000000, 1.000000000000000000, 0.000000000000000000 ) ) ;
#14317 = VERTEX_POINT ( 'NONE', #18619 ) ;
#14318 = CARTESIAN_POINT ( 'NONE',  ( -1.536366799937282313, 29.95086340285667603, 1.999167105995454552 ) ) ;
#14319 = B_SPLINE_CURVE_WITH_KNOTS ( 'NONE', 3,
 ( #19650, #21590, #13821, #16110, #19403, #23261, #2935, #19887, #8511, #15987, #1479, #21461, #14318, #23379, #6797, #5004, #10197, #2817 ),
 .UNSPECIFIED., .F., .F.,
 ( 4, 2, 2, 2, 2, 2, 2, 2, 4 ),
 ( 0.000000000000000000, 0.1250000000000000000, 0.2500000000000000000, 0.3750000000000000000, 0.5000000000000000000, 0.6250000000000000000, 0.7500000000000000000, 0.8750000000000000000, 1.000000000000000000 ),
 .UNSPECIFIED. ) ;
#14320 = CARTESIAN_POINT ( 'NONE',  ( -24.50000000000000000, 7.216878364870000340, 12.50000000000000000 ) ) ;
#14321 = CARTESIAN_POINT ( 'NONE',  ( 0.000000000000000000, 9.100092063578999912, -1.999999999999988676 ) ) ;
#14322 = VERTEX_POINT ( 'NONE', #7464 ) ;
#14323 = EDGE_CURVE ( 'NONE', #3318, #9734, #6005, .T. ) ;
#14324 = CARTESIAN_POINT ( 'NONE',  ( -20.94728937253999845, -10.43362079082000093, 2.366296559912000053 ) ) ;
#14325 = EDGE_CURVE ( 'NONE', #1, #16256, #20553, .T. ) ;
#14326 = CARTESIAN_POINT ( 'NONE',  ( 23.99478584078000054, 7.550251870592999737, -11.73017644753999988 ) ) ;
#14327 = CARTESIAN_POINT ( 'NONE',  ( 15.02841901554468684, 9.563305402470449579, 3.947719917943012025 ) ) ;
#14328 = DIRECTION ( 'NONE',  ( 1.000000000000000000, 0.000000000000000000, 0.000000000000000000 ) ) ;
#14329 = CARTESIAN_POINT ( 'NONE',  ( 18.68066617734999824, 0.006293508795006000009, 10.66027559447000073 ) ) ;
#14330 = CARTESIAN_POINT ( 'NONE',  ( 1.375818737057000085, 30.26428676817999985, 1.918154343084000013 ) ) ;
#14331 = CARTESIAN_POINT ( 'NONE',  ( 13.60016193201688139, 6.912966986891127874, -5.794099676471392790 ) ) ;
#14332 = CARTESIAN_POINT ( 'NONE',  ( -4.574431393056000772, 12.47762465527999076, -1.200270365199999523 ) ) ;
#14333 = VERTEX_POINT ( 'NONE', #13161 ) ;
#14334 = CARTESIAN_POINT ( 'NONE',  ( -21.95942920454664815, -4.650705262963104047, -8.069294568062584716 ) ) ;
#14335 = ORIENTED_EDGE ( 'NONE', *, *, #19884, .F. ) ;
#14336 = CARTESIAN_POINT ( 'NONE',  ( 0.000000000000000000, 28.00000000000000000, 0.000000000000000000 ) ) ;
#14337 = CARTESIAN_POINT ( 'NONE',  ( 24.50000000000000000, -9.344098705406999272, -3.489386534399999906 ) ) ;
#14338 = ORIENTED_EDGE ( 'NONE', *, *, #20674, .F. ) ;
#14339 = DIRECTION ( 'NONE',  ( 0.000000000000000000, -1.000000000000000000, 0.000000000000000000 ) ) ;
#14340 = FACE_BOUND ( 'NONE', #16242, .T. ) ;
#14341 = CARTESIAN_POINT ( 'NONE',  ( 24.36165043081789960, 3.174800876238617953, -12.50000000000000000 ) ) ;
#14342 = ORIENTED_EDGE ( 'NONE', *, *, #10548, .F. ) ;
#14343 = CARTESIAN_POINT ( 'NONE',  ( -11.33465399291999987, 5.498006771546000593, 13.43624142368999941 ) ) ;
#14344 = FACE_OUTER_BOUND ( 'NONE', #13846, .T. ) ;
#14345 = CARTESIAN_POINT ( 'NONE',  ( 2.000000000000198508, 24.49999999999999645, -3.464101615138341028 ) ) ;
#14346 = ORIENTED_EDGE ( 'NONE', *, *, #17780, .T. ) ;
#14347 = DIRECTION ( 'NONE',  ( -1.000000000000000000, 0.000000000000000000, 0.000000000000000000 ) ) ;
#14348 = CARTESIAN_POINT ( 'NONE',  ( 20.99977027363030047, -10.24898389550873290, 2.455023892489411885 ) ) ;
#14349 = CARTESIAN_POINT ( 'NONE',  ( -13.99999999999999467, -0.2201081049113881583, 9.776473952568711212 ) ) ;
#14350 = CARTESIAN_POINT ( 'NONE',  ( 16.25882916898783392, -0.6197948286024473896, -10.35986595345727146 ) ) ;
#14351 = CARTESIAN_POINT ( 'NONE',  ( -4.886147650005925769, 13.44678367007931818, 5.723089997228743009 ) ) ;
#14352 = CARTESIAN_POINT ( 'NONE',  ( -2.340764093348000063, 30.20884863804000275, -0.1017020371176000082 ) ) ;
#14353 = AXIS2_PLACEMENT_3D ( 'NONE', #1800, #7361, #11123 ) ;
#14354 = CARTESIAN_POINT ( 'NONE',  ( -18.60180781823000018, -9.793299576559000741, 0.7034231180304000297 ) ) ;
#14355 = CARTESIAN_POINT ( 'NONE',  ( 0.8827757939797101772, 29.95033105760662906, -1.971174946009011553 ) ) ;
#14356 = ORIENTED_EDGE ( 'NONE', *, *, #7178, .T. ) ;
#14357 = CARTESIAN_POINT ( 'NONE',  ( 23.47552080277744935, -4.670392666604991305, 8.100843789317771382 ) ) ;
#14358 = CARTESIAN_POINT ( 'NONE',  ( 11.53663804755082190, 12.55807338460112454, -3.248594360998799502 ) ) ;
#14359 = DIRECTION ( 'NONE',  ( 0.000000000000000000, 1.000000000000000000, 0.000000000000000000 ) ) ;
#14360 = CARTESIAN_POINT ( 'NONE',  ( -0.9262738205379743572, 23.62802189508158790, -1.915861982203995284 ) ) ;
#14361 = ORIENTED_EDGE ( 'NONE', *, *, #15236, .F. ) ;
#14362 = CARTESIAN_POINT ( 'NONE',  ( 24.07420734439589083, -7.985988878874604069, -11.16786151310754960 ) ) ;
#14363 = CARTESIAN_POINT ( 'NONE',  ( 2.500000000000000000, 18.50000000000000000, 0.000000000000000000 ) ) ;
#14364 = CARTESIAN_POINT ( 'NONE',  ( 2.398621549960997967, 11.68146935173001033, -4.243417778616998426 ) ) ;
#14365 = EDGE_LOOP ( 'NONE', ( #4924, #10974, #7968, #12467, #2486 ) ) ;
#14366 = CARTESIAN_POINT ( 'NONE',  ( 18.19293875730999943, -2.463108239980999592, 8.917637382198998708 ) ) ;
#14367 = ORIENTED_EDGE ( 'NONE', *, *, #11634, .F. ) ;
#14368 = CARTESIAN_POINT ( 'NONE',  ( 1.890284010598150877, 26.36143429054256870, 1.130219607317671127 ) ) ;
#14369 = SHAPE_DEFINITION_REPRESENTATION ( #8047, #8755 ) ;
#14370 = DIRECTION ( 'NONE',  ( 0.000000000000000000, -1.000000000000000000, 0.000000000000000000 ) ) ;
#14371 = ORIENTED_EDGE ( 'NONE', *, *, #22806, .T. ) ;
#14372 = DIRECTION ( 'NONE',  ( 0.7071067811866525998, 0.000000000000000000, -0.7071067811864425456 ) ) ;
#14373 = CARTESIAN_POINT ( 'NONE',  ( -4.792894583204066805, 15.72849393113409633, -3.814013712966466407 ) ) ;
#14374 = CARTESIAN_POINT ( 'NONE',  ( -21.91931851383999685, -0.7111562311954999771, 10.62484833929000061 ) ) ;
#14375 = CARTESIAN_POINT ( 'NONE',  ( -17.99572818580000089, -1.813981674565000146, -9.633252329321001284 ) ) ;
#14376 = CARTESIAN_POINT ( 'NONE',  ( -4.850296048403001770, 13.26922248379001523, -5.932245385413001948 ) ) ;
#14377 = CARTESIAN_POINT ( 'NONE',  ( -22.74900695987042099, -4.110693411953544540, -9.728987031145388542 ) ) ;
#14378 = CARTESIAN_POINT ( 'NONE',  ( 1.767919490126756310, 26.52540550784508611, 1.264046928454615193 ) ) ;
#14379 = DIRECTION ( 'NONE',  ( -1.000000000000000000, 0.000000000000000000, 0.000000000000000000 ) ) ;
#14380 = EDGE_CURVE ( 'NONE', #8826, #4536, #7831, .T. ) ;
#14381 = CARTESIAN_POINT ( 'NONE',  ( 2.066176616758256035, 30.64207483863886594, -0.6409079810234022956 ) ) ;
#14382 = EDGE_LOOP ( 'NONE', ( #7207, #16965, #17703, #14417 ) ) ;
#14383 = FACE_OUTER_BOUND ( 'NONE', #10595, .T. ) ;
#14384 = CARTESIAN_POINT ( 'NONE',  ( -2.104626470933999904, 26.17913313895000016, -1.289728978252000058 ) ) ;
#14385 = AXIS2_PLACEMENT_3D ( 'NONE', #18357, #11220, #12897 ) ;
#14386 = CARTESIAN_POINT ( 'NONE',  ( 4.829987487923999900, 14.79876397742000016, -3.766541047082999860 ) ) ;
#14387 = CARTESIAN_POINT ( 'NONE',  ( -1.796659635434000091, 27.91771896306000045, 1.416372250270000022 ) ) ;
#14388 = CARTESIAN_POINT ( 'NONE',  ( -3.673647344300186468, 12.04674575989788465, 3.146065391725001881 ) ) ;
#14389 = ORIENTED_EDGE ( 'NONE', *, *, #19768, .T. ) ;
#14390 = CARTESIAN_POINT ( 'NONE',  ( -10.90000000000000036, 1.358133300253999998E-14, 0.000000000000000000 ) ) ;
#14391 = CARTESIAN_POINT ( 'NONE',  ( 4.834782059083999606, 12.44497316928999808, -0.3759403457470999466 ) ) ;
#14392 = EDGE_CURVE ( 'NONE', #19829, #5746, #19411, .T. ) ;
#14393 = CARTESIAN_POINT ( 'NONE',  ( 24.26191870746986012, 6.808678168838079969, -6.906054575474446011 ) ) ;
#14394 = CARTESIAN_POINT ( 'NONE',  ( -2.153985071724999756, 30.83999999999999986, 0.1610847937796999751 ) ) ;
#14395 = VERTEX_POINT ( 'NONE', #18851 ) ;
#14396 = FACE_OUTER_BOUND ( 'NONE', #8763, .T. ) ;
#14397 = DIRECTION ( 'NONE',  ( -1.000000000000000000, 0.000000000000000000, 0.000000000000000000 ) ) ;
#14398 = CARTESIAN_POINT ( 'NONE',  ( 12.40593892130999976, 9.405156509668998410, -1.966610333673999955 ) ) ;
#14399 = CARTESIAN_POINT ( 'NONE',  ( 18.72471403812598467, 8.467466865290406375, 6.090674659130430157 ) ) ;
#14400 = ORIENTED_EDGE ( 'NONE', *, *, #7702, .F. ) ;
#14401 = DIRECTION ( 'NONE',  ( 0.000000000000000000, 0.7071067811866525998, -0.7071067811864425456 ) ) ;
#14402 = CARTESIAN_POINT ( 'NONE',  ( -6.042815982636000172, 21.50000000000000000, -1.000000000000000000 ) ) ;
#14403 = CARTESIAN_POINT ( 'NONE',  ( 18.50983580085999947, 11.40398223831000024, 0.8544022015744000553 ) ) ;
#14404 = CARTESIAN_POINT ( 'NONE',  ( 13.50000000000000533, -6.340245170342347691, 7.979342322378518482 ) ) ;
#14405 = VERTEX_POINT ( 'NONE', #3966 ) ;
#14406 = DIRECTION ( 'NONE',  ( 0.000000000000000000, 1.000000000000000000, 0.000000000000000000 ) ) ;
#14407 = CARTESIAN_POINT ( 'NONE',  ( 24.55082877617000037, -5.845823156057000425, 8.945057363882000345 ) ) ;
#14408 = EDGE_CURVE ( 'NONE', #20281, #7389, #6969, .T. ) ;
#14409 = CARTESIAN_POINT ( 'NONE',  ( -23.95278192272984086, -1.063754273011168205, 9.723242869295845026 ) ) ;
#14410 = CARTESIAN_POINT ( 'NONE',  ( 13.61158555497621947, -7.958227948172696742, 6.606147741580802979 ) ) ;
#14411 = CARTESIAN_POINT ( 'NONE',  ( -3.978825713501787931, 13.87455081233140497, 4.851109908756392919 ) ) ;
#14412 = CARTESIAN_POINT ( 'NONE',  ( -4.573911348824003298, 12.37758549377001671, 1.892950700447998402 ) ) ;
#14413 = DIRECTION ( 'NONE',  ( 0.000000000000000000, 1.000000000000000000, 0.000000000000000000 ) ) ;
#14414 = ORIENTED_EDGE ( 'NONE', *, *, #4520, .T. ) ;
#14415 = FACE_OUTER_BOUND ( 'NONE', #15179, .T. ) ;
#14416 = CARTESIAN_POINT ( 'NONE',  ( 1.709378212513718687, 12.94272856688811046, 1.056191457993780114 ) ) ;
#14417 = ORIENTED_EDGE ( 'NONE', *, *, #16936, .T. ) ;
#14418 = CARTESIAN_POINT ( 'NONE',  ( 2.301266907105999682, 25.82233687760000151, 0.4915126353211999866 ) ) ;
#14419 = DIRECTION ( 'NONE',  ( 0.000000000000000000, -1.000000000000000000, 0.000000000000000000 ) ) ;
#14420 = EDGE_CURVE ( 'NONE', #23795, #6008, #22709, .T. ) ;
#14421 = CARTESIAN_POINT ( 'NONE',  ( 12.06371966923812522, -5.117452910095027896, -12.50009924164533182 ) ) ;
#14422 = VECTOR ( 'NONE', #13817, 1000.000000000000000 ) ;
#14423 = CARTESIAN_POINT ( 'NONE',  ( 19.58133333333332970, 3.621958592900809126, 8.534357609150490021 ) ) ;
#14424 = DIRECTION ( 'NONE',  ( 0.000000000000000000, 0.7071067811866525998, -0.7071067811864425456 ) ) ;
#14425 = VERTEX_POINT ( 'NONE', #13880 ) ;
#14426 = CARTESIAN_POINT ( 'NONE',  ( 0.000000000000000000, 24.50000000000000000, 0.000000000000000000 ) ) ;
#14427 = PLANE ( 'NONE',  #14784 ) ;
#14428 = DIRECTION ( 'NONE',  ( 0.000000000000000000, 1.000000000000000000, 0.000000000000000000 ) ) ;
#14429 = ORIENTED_EDGE ( 'NONE', *, *, #2403, .T. ) ;
#14430 = CARTESIAN_POINT ( 'NONE',  ( -20.09045569450000102, 9.845892643941999367, -4.125506862962999399 ) ) ;
#14431 = CARTESIAN_POINT ( 'NONE',  ( 0.7621399210758000864, 23.93675694115000141, 2.004617982535000120 ) ) ;
#14432 = CARTESIAN_POINT ( 'NONE',  ( 14.60105817408460638, 4.787368022142956647, -9.159926853143835146 ) ) ;
#14433 = CARTESIAN_POINT ( 'NONE',  ( -7.834000000000000519, 10.59999999999999964, 0.000000000000000000 ) ) ;
#14434 = CARTESIAN_POINT ( 'NONE',  ( 20.45495348602999997, 1.509263456234000156, 11.10181671682000015 ) ) ;
#14435 = EDGE_CURVE ( 'NONE', #21280, #1169, #4954, .T. ) ;
#14436 = CARTESIAN_POINT ( 'NONE',  ( 0.5645359770996000170, 30.65695694114999981, -2.093200898226000195 ) ) ;
#14437 = CARTESIAN_POINT ( 'NONE',  ( 13.60079008836671477, 6.926023288026004643, -5.778502639464679014 ) ) ;
#14438 = EDGE_CURVE ( 'NONE', #15451, #19406, #594, .T. ) ;
#14439 = CARTESIAN_POINT ( 'NONE',  ( -6.504405627207126450, 15.46487054860210364, -1.467966815537356196 ) ) ;
#14440 = AXIS2_PLACEMENT_3D ( 'NONE', #22510, #4441, #11831 ) ;
#14441 = CARTESIAN_POINT ( 'NONE',  ( -21.73267920454664903, 2.415784607553221441, -8.988730734449054793 ) ) ;
#14442 = VERTEX_POINT ( 'NONE', #19082 ) ;
#14443 = FACE_OUTER_BOUND ( 'NONE', #15464, .T. ) ;
#14444 = DIRECTION ( 'NONE',  ( 0.000000000000000000, 0.000000000000000000, 1.000000000000000000 ) ) ;
#14445 = VERTEX_POINT ( 'NONE', #8197 ) ;
#14446 = FACE_OUTER_BOUND ( 'NONE', #2231, .T. ) ;
#14447 = CARTESIAN_POINT ( 'NONE',  ( 17.01429166666665083, 1.192094632364767870, -9.107901970610145170 ) ) ;
#14448 = EDGE_CURVE ( 'NONE', #21878, #22057, #22725, .T. ) ;
#14449 = CARTESIAN_POINT ( 'NONE',  ( 2.750000000000000000, 24.29999999999999716, 0.000000000000000000 ) ) ;
#14450 = ADVANCED_FACE ( 'NONE', ( #8442 ), #6616, .F. ) ;
#14451 = CARTESIAN_POINT ( 'NONE',  ( 18.44875144328999994, 10.74386948049999901, 2.882141228404999644 ) ) ;
#14452 = ORIENTED_EDGE ( 'NONE', *, *, #3651, .T. ) ;
#14453 = CARTESIAN_POINT ( 'NONE',  ( -9.385278638770000015, -0.05147163365328999429, -15.21832980031999938 ) ) ;
#14454 = CARTESIAN_POINT ( 'NONE',  ( 13.50000000000000000, 5.478253366763097709, 8.484493166734903724 ) ) ;
#14455 = LINE ( 'NONE', #20271, #10970 ) ;
#14456 = ORIENTED_EDGE ( 'NONE', *, *, #16439, .F. ) ;
#14457 = PRESENTATION_STYLE_ASSIGNMENT (( #20037 ) ) ;
#14458 = CARTESIAN_POINT ( 'NONE',  ( 21.91162244696776540, 10.46836026662980679, -2.349396852667112956 ) ) ;
#14459 = CARTESIAN_POINT ( 'NONE',  ( -2.944270284434495899, 26.42936170367566362, 2.918926912232258530 ) ) ;
#14460 = CARTESIAN_POINT ( 'NONE',  ( 16.10403698457205834, -5.878893883532452236, -8.533248856027976004 ) ) ;
#14461 = B_SPLINE_CURVE_WITH_KNOTS ( 'NONE', 3,
 ( #17018, #6234, #20654, #9996, #15433, #22698, #11816, #13615, #21013, #17385, #782, #11579, #11459, #17259, #14949, #18955, #9513, #4425 ),
 .UNSPECIFIED., .F., .F.,
 ( 4, 2, 2, 2, 2, 2, 2, 2, 4 ),
 ( 0.000000000000000000, 0.1250000000000000555, 0.2500000000000000555, 0.3750000000000000555, 0.5000000000000000000, 0.6249999999999998890, 0.7499999999999998890, 0.8749999999999998890, 1.000000000000000000 ),
 .UNSPECIFIED. ) ;
#14462 = CARTESIAN_POINT ( 'NONE',  ( -4.900699999999999612, 1.284663064832999817E-14, 0.000000000000000000 ) ) ;
#14463 = AXIS2_PLACEMENT_3D ( 'NONE', #3241, #21522, #12082 ) ;
#14464 = CARTESIAN_POINT ( 'NONE',  ( 1.463530596214999813, 29.93944235804000087, -1.626872480619000028 ) ) ;
#14465 = UNCERTAINTY_MEASURE_WITH_UNIT (LENGTH_MEASURE( 1.000000000000000082E-05 ), #11147, 'distance_accuracy_value', 'NONE');
#14466 = CARTESIAN_POINT ( 'NONE',  ( -18.43943555148999991, -2.412201287215999912, -10.06532802039999908 ) ) ;
#14467 = CARTESIAN_POINT ( 'NONE',  ( 1.411316182247830175, 29.91300950840242479, -1.635672673209419559 ) ) ;
#14468 = ORIENTED_EDGE ( 'NONE', *, *, #19568, .T. ) ;
#14469 = CARTESIAN_POINT ( 'NONE',  ( -24.33938584177210984, -2.815218398150926671, 12.49992678696526127 ) ) ;
#14470 = CARTESIAN_POINT ( 'NONE',  ( 19.44804762184721270, -10.50094980715322635, 0.1342334127711540259 ) ) ;
#14471 = FACE_OUTER_BOUND ( 'NONE', #15723, .T. ) ;
#14472 = B_SPLINE_CURVE_WITH_KNOTS ( 'NONE', 3,
 ( #13602, #17367, #4409, #19180, #4170, #2589, #18943, #768, #13724, #21122 ),
 .UNSPECIFIED., .F., .F.,
 ( 4, 2, 2, 2, 4 ),
 ( 0.000000000000000000, 0.2500000000000001110, 0.5000000000000001110, 0.7500000000000001110, 1.000000000000000000 ),
 .UNSPECIFIED. ) ;
#14473 = AXIS2_PLACEMENT_3D ( 'NONE', #18442, #2196, #11299 ) ;
#14474 = VERTEX_POINT ( 'NONE', #4438 ) ;
#14475 = SHAPE_REPRESENTATION ( 'Ball Seat Ring', ( #4390 ), #20254 ) ;
#14476 = CARTESIAN_POINT ( 'NONE',  ( 24.34804274388851297, -9.160073233599486997, -9.134287758352421349 ) ) ;
#14477 = CARTESIAN_POINT ( 'NONE',  ( 4.926165394784816520, 14.31396120642910930, -3.835254638722358500 ) ) ;
#14478 = CARTESIAN_POINT ( 'NONE',  ( -4.917002979092000459, 12.44024335427998906, -0.01122529268158000207 ) ) ;
#14479 = ORIENTED_EDGE ( 'NONE', *, *, #13633, .F. ) ;
#14480 = DIRECTION ( 'NONE',  ( 0.000000000000000000, 1.000000000000000000, 0.000000000000000000 ) ) ;
#14481 = CIRCLE ( 'NONE', #2098, 15.43375672974000068 ) ;
#14482 = ORIENTED_EDGE ( 'NONE', *, *, #23448, .F. ) ;
#14483 = CARTESIAN_POINT ( 'NONE',  ( -4.123153084920957667, 15.07815051851633825, 4.529465602894293674 ) ) ;
#14484 = CARTESIAN_POINT ( 'NONE',  ( -1.536366799937282090, 29.71666666666667211, 1.999167105995454552 ) ) ;
#14485 = ORIENTED_EDGE ( 'NONE', *, *, #9923, .F. ) ;
#14486 = CARTESIAN_POINT ( 'NONE',  ( -15.15692920454666570, -7.916761560459355529, 4.562790735126731612 ) ) ;
#14487 = AXIS2_PLACEMENT_3D ( 'NONE', #8423, #13734, #13858 ) ;
#14488 = CARTESIAN_POINT ( 'NONE',  ( -19.67110492428000157, -10.05584626669999970, 0.0004483298532730999866 ) ) ;
#14489 = DIRECTION ( 'NONE',  ( 0.000000000000000000, -1.000000000000000000, 0.000000000000000000 ) ) ;
#14490 = CARTESIAN_POINT ( 'NONE',  ( 18.63933333333331888, -4.608031391969340085, -7.994750628324704955 ) ) ;
#14491 = CARTESIAN_POINT ( 'NONE',  ( -22.77474208561820390, -4.966028226955915947, -9.323134938704122021 ) ) ;
#14492 = CARTESIAN_POINT ( 'NONE',  ( 0.6990180580869200799, 26.44590205212557521, 2.094941974207407132 ) ) ;
#14493 = VECTOR ( 'NONE', #12516, 1000.000000000000000 ) ;
#14494 = FACE_OUTER_BOUND ( 'NONE', #21220, .T. ) ;
#14495 = CARTESIAN_POINT ( 'NONE',  ( 1.509965525092430205, 30.70526206248454670, -1.547206845526075236 ) ) ;
#14496 = EDGE_LOOP ( 'NONE', ( #5802, #19080, #3779, #1542, #8458 ) ) ;
#14497 = CARTESIAN_POINT ( 'NONE',  ( -17.42442920454667998, 4.592095577738842138, 7.967605896327013326 ) ) ;
#14498 = CARTESIAN_POINT ( 'NONE',  ( 2.258737362907614621, 26.35873736869804773, 0.2437184634590501553 ) ) ;
#14499 = CARTESIAN_POINT ( 'NONE',  ( 1.350549796471707253, 24.78453005107567009, 1.633252776670135908 ) ) ;
#14500 = CARTESIAN_POINT ( 'NONE',  ( 1.416372250270000022, 26.74771896305999874, -1.796659635434000091 ) ) ;
#14501 = VECTOR ( 'NONE', #8359, 1000.000000000000000 ) ;
#14502 = CARTESIAN_POINT ( 'NONE',  ( 2.418195492079564968, 11.72965300045306414, 4.174376928245445484 ) ) ;
#14503 = ORIENTED_EDGE ( 'NONE', *, *, #22210, .F. ) ;
#14504 = CARTESIAN_POINT ( 'NONE',  ( -1.969571242956765111, 11.64777130037908393, -4.396811160587570377 ) ) ;
#14505 = CARTESIAN_POINT ( 'NONE',  ( 2.000000000000000000, 28.00000000000000000, 3.464101615137999968 ) ) ;
#14506 = CARTESIAN_POINT ( 'NONE',  ( 1.414363803402227227, 6.923393381151994319, 1.035861679437342753 ) ) ;
#14507 = ORIENTED_EDGE ( 'NONE', *, *, #12143, .F. ) ;
#14508 = EDGE_CURVE ( 'NONE', #5518, #7680, #19087, .T. ) ;
#14509 = CARTESIAN_POINT ( 'NONE',  ( 1.999167105995466764, 24.31666666666666643, 1.536366799937266325 ) ) ;
#14510 = DIRECTION ( 'NONE',  ( 0.000000000000000000, -1.000000000000000000, 0.000000000000000000 ) ) ;
#14511 = CARTESIAN_POINT ( 'NONE',  ( 15.80625142131000160, 5.282396774718000287, -8.133049213409000444 ) ) ;
#14512 = CARTESIAN_POINT ( 'NONE',  ( 18.69530137406649928, 9.024773782881792883, 5.230709212474926595 ) ) ;
#14513 = UNCERTAINTY_MEASURE_WITH_UNIT (LENGTH_MEASURE( 1.000000000000000082E-05 ), #4478, 'distance_accuracy_value', 'NONE');
#14514 = DIRECTION ( 'NONE',  ( 0.000000000000000000, -1.000000000000000000, 0.000000000000000000 ) ) ;
#14515 = CARTESIAN_POINT ( 'NONE',  ( -1.169337612399999893, 30.82072358173000381, -1.691178548922000147 ) ) ;
#14516 = CARTESIAN_POINT ( 'NONE',  ( 17.49421080085999947, -10.89330037972999854, 3.387123339711000103 ) ) ;
#14517 = DIRECTION ( 'NONE',  ( -0.9999999999922942751, 3.925717498811976060E-06, 6.459656137320962354E-09 ) ) ;
#14518 = AXIS2_PLACEMENT_3D ( 'NONE', #15611, #19011, #7879 ) ;
#14519 = VERTEX_POINT ( 'NONE', #15565 ) ;
#14520 = CARTESIAN_POINT ( 'NONE',  ( 0.000000000000000000, 31.00000000000000000, -2.000000000000000000 ) ) ;
#14521 = CARTESIAN_POINT ( 'NONE',  ( 21.63524950958999682, -9.258690811328998294, -5.498005089659000255 ) ) ;
#14522 = EDGE_CURVE ( 'NONE', #11598, #10311, #11711, .T. ) ;
#14523 = CARTESIAN_POINT ( 'NONE',  ( -24.17459695600129876, 8.825400305006976254, 4.719873724747784216 ) ) ;
#14524 = DIRECTION ( 'NONE',  ( 0.000000000000000000, -1.000000000000000000, 0.000000000000000000 ) ) ;
#14525 = CARTESIAN_POINT ( 'NONE',  ( -3.898965866421516324, 13.96122025683682288, 4.845918179761490308 ) ) ;
#14526 = CARTESIAN_POINT ( 'NONE',  ( 4.940723035539999586, 12.51282731614000276, -0.1566769263144998925 ) ) ;
#14527 = CARTESIAN_POINT ( 'NONE',  ( 2.649999999999999911, 26.50000000000000000, 0.000000000000000000 ) ) ;
#14528 = EDGE_LOOP ( 'NONE', ( #1646, #20530, #23566, #9768, #13877 ) ) ;
#14529 = CARTESIAN_POINT ( 'NONE',  ( 2.325656998026726541, 30.67434301629538851, 0.4535295980105740199 ) ) ;
#14530 = CARTESIAN_POINT ( 'NONE',  ( -4.000000000000000000, 26.41693820796410108, 1.184172465503444904 ) ) ;
#14531 = ORIENTED_EDGE ( 'NONE', *, *, #6857, .F. ) ;
#14532 = CARTESIAN_POINT ( 'NONE',  ( -0.8187353038599000099, 24.39316693604000008, -2.000180504622000033 ) ) ;
#14533 = CARTESIAN_POINT ( 'NONE',  ( 5.428958415689999484, 14.69816721964000195, 2.857937668952999832 ) ) ;
#14534 = CARTESIAN_POINT ( 'NONE',  ( 2.000000000000000000, 23.00000000000000000, 0.000000000000000000 ) ) ;
#14535 = CARTESIAN_POINT ( 'NONE',  ( 19.45483333333332610, 6.898272746453336879, 6.189253307314870334 ) ) ;
#14536 = CARTESIAN_POINT ( 'NONE',  ( -0.6543697108982037269, 27.83333333333333925, -2.434931691670788823 ) ) ;
#14537 = EDGE_CURVE ( 'NONE', #7164, #1236, #21396, .T. ) ;
#14538 = LINE ( 'NONE', #12499, #17125 ) ;
#14539 = ORIENTED_EDGE ( 'NONE', *, *, #7041, .F. ) ;
#14540 = DIRECTION ( 'NONE',  ( 0.000000000000000000, -1.000000000000000000, 0.000000000000000000 ) ) ;
#14541 = CARTESIAN_POINT ( 'NONE',  ( -1.842949095694737638, 26.21789781124859786, 1.045490242349867982 ) ) ;
#14542 = DIRECTION ( 'NONE',  ( 1.000000000000000000, 0.000000000000000000, 0.000000000000000000 ) ) ;
#14543 = ORIENTED_EDGE ( 'NONE', *, *, #4962, .T. ) ;
#14544 = CARTESIAN_POINT ( 'NONE',  ( -20.84844433051999957, -6.396441138360000167, -9.216716464522999530 ) ) ;
#14545 = CARTESIAN_POINT ( 'NONE',  ( 2.291512794585000012, 25.56043239939999978, 0.4488570629504000098 ) ) ;
#14546 = CARTESIAN_POINT ( 'NONE',  ( 14.66409083246537470, 6.614115962116787095, -7.929118690434196814 ) ) ;
#14547 = DIRECTION ( 'NONE',  ( -1.000000000000000000, 0.000000000000000000, 0.000000000000000000 ) ) ;
#14548 = CARTESIAN_POINT ( 'NONE',  ( 20.74819667979999949, 1.510347020690999909, 11.10979287247999991 ) ) ;
#14549 = CARTESIAN_POINT ( 'NONE',  ( -1.795908923730999751, 30.69514008176999909, -1.532003524410999962 ) ) ;
#14550 = EDGE_CURVE ( 'NONE', #8738, #20461, #796, .T. ) ;
#14551 = CARTESIAN_POINT ( 'NONE',  ( 13.98171503422127238, 7.305407177158877552, 5.378490655644252882 ) ) ;
#14552 = FACE_OUTER_BOUND ( 'NONE', #1467, .T. ) ;
#14553 = VECTOR ( 'NONE', #15519, 1000.000000000000000 ) ;
#14554 = LINE ( 'NONE', #21947, #15247 ) ;
#14555 = EDGE_LOOP ( 'NONE', ( #14224, #17632, #1176, #13532 ) ) ;
#14556 = CARTESIAN_POINT ( 'NONE',  ( -15.00576253787999903, -9.056359154562001024, 0.000000000000000000 ) ) ;
#14557 = CYLINDRICAL_SURFACE ( 'NONE', #4576, 3.000000000000000000 ) ;
#14558 = B_SPLINE_CURVE_WITH_KNOTS ( 'NONE', 3,
 ( #5055, #20054, #3691, #8800, #1532, #12886, #16162, #7087, #14477, #12551, #19936, #10618, #23564, #3580, #49, #20287, #22098, #3470, #1642, #3355, #20172, #10734, #16400, #9029, #14589 ),
 .UNSPECIFIED., .F., .F.,
 ( 4, 2, 2, 1, 2, 2, 2, 2, 1, 1, 2, 2, 2, 4 ),
 ( 0.000000000000000000, 0.2499999999999427125, 0.3749999999999121258, 0.4374999999998951949, 0.4687499999998844813, 0.4999999999998737676, 0.6249999999998363531, 0.6874999999998204769, 0.7187499999998154809, 0.7343749999998131495, 0.7421874999998120392, 0.7499999999998109290, 0.8749999999999055200, 1.000000000000000000 ),
 .UNSPECIFIED. ) ;
#14559 = ADVANCED_FACE ( 'NONE', ( #2495 ), #8438, .T. ) ;
#14560 = VERTEX_POINT ( 'NONE', #8079 ) ;
#14561 = CARTESIAN_POINT ( 'NONE',  ( 21.72020603379665360, 2.415700825681953656, 8.988418979289773958 ) ) ;
#14562 = CIRCLE ( 'NONE', #5305, 13.77250448648999637 ) ;
#14563 = FACE_OUTER_BOUND ( 'NONE', #19814, .T. ) ;
#14564 = CARTESIAN_POINT ( 'NONE',  ( -14.39083492636570583, 4.156485310037820291, 9.484860138480087244 ) ) ;
#14565 = EDGE_CURVE ( 'NONE', #22702, #13196, #21427, .T. ) ;
#14566 = EDGE_CURVE ( 'NONE', #15625, #13107, #1863, .T. ) ;
#14567 = ORIENTED_EDGE ( 'NONE', *, *, #21326, .F. ) ;
#14568 = VECTOR ( 'NONE', #21725, 1000.000000000000000 ) ;
#14569 = CARTESIAN_POINT ( 'NONE',  ( -11.93821506584999881, 12.87565757039999959, -7.434806685507000523 ) ) ;
#14570 = CARTESIAN_POINT ( 'NONE',  ( 13.49999999999999822, 5.804425006068715476, 8.246010899024623697 ) ) ;
#14571 = CARTESIAN_POINT ( 'NONE',  ( -14.38789236265223437, -12.88903867673619885, -2.675117728967849384 ) ) ;
#14572 = ORIENTED_EDGE ( 'NONE', *, *, #11189, .T. ) ;
#14573 = CARTESIAN_POINT ( 'NONE',  ( 20.47030772137050647, 5.028569603156692658, 9.244401094538714503 ) ) ;
#14574 = FACE_OUTER_BOUND ( 'NONE', #7821, .T. ) ;
#14575 = CARTESIAN_POINT ( 'NONE',  ( 15.97284269412691060, -9.008167718500386556, -5.113775645086368726 ) ) ;
#14576 = DIRECTION ( 'NONE',  ( 1.127781618093000070E-10, -1.517612146120235195E-19, -1.000000000000000000 ) ) ;
#14577 = CARTESIAN_POINT ( 'NONE',  ( 1.571106264104000116, 30.73074958545000257, -1.523240044125999892 ) ) ;
#14578 = EDGE_CURVE ( 'NONE', #953, #8305, #20914, .T. ) ;
#14579 = VECTOR ( 'NONE', #7897, 1000.000000000000000 ) ;
#14581 = AXIS2_PLACEMENT_3D ( 'NONE', #4109, #18649, #11387 ) ;
#14580 = CARTESIAN_POINT ( 'NONE',  ( -4.000000000000000000, 28.30000000000000071, -2.309401076759000304 ) ) ;
#14582 = CARTESIAN_POINT ( 'NONE',  ( 0.8902908324380954808, 29.94984802629786813, -1.967793501657690403 ) ) ;
#14583 = ORIENTED_EDGE ( 'NONE', *, *, #5938, .F. ) ;
#14584 = CARTESIAN_POINT ( 'NONE',  ( -1.271343851483999865, 23.71194070365999806, -1.772672411470999965 ) ) ;
#14585 = CARTESIAN_POINT ( 'NONE',  ( 20.38436928271863025, 10.48308585629694711, 0.9317613066503177555 ) ) ;
#14586 = CARTESIAN_POINT ( 'NONE',  ( -0.8942398442040443429, 23.65531290036175704, -1.961072913851835242 ) ) ;
#14587 = ORIENTED_EDGE ( 'NONE', *, *, #10473, .F. ) ;
#14588 = CARTESIAN_POINT ( 'NONE',  ( 0.000000000000000000, 7.049999902385000183, 0.000000000000000000 ) ) ;
#14589 = CARTESIAN_POINT ( 'NONE',  ( 4.829987487923999900, 14.79876397742000016, -3.766541047082999860 ) ) ;
#14590 = CARTESIAN_POINT ( 'NONE',  ( -4.466956411286998829, 12.27369686073000032, -2.063459869057001406 ) ) ;
#14591 = ORIENTED_EDGE ( 'NONE', *, *, #22878, .T. ) ;
#14592 = EDGE_CURVE ( 'NONE', #14519, #20964, #10761, .T. ) ;
#14593 = CARTESIAN_POINT ( 'NONE',  ( 0.000000000000000000, 15.09999999999999964, 0.000000000000000000 ) ) ;
#14594 = EDGE_CURVE ( 'NONE', #11381, #19819, #6088, .T. ) ;
#14595 = ORIENTED_EDGE ( 'NONE', *, *, #22115, .F. ) ;
#14596 = VECTOR ( 'NONE', #825, 1000.000000000000000 ) ;
#14597 = CARTESIAN_POINT ( 'NONE',  ( -2.499999999999999556, 28.25086340285665543, 0.3272492347489435738 ) ) ;
#14598 = DIRECTION ( 'NONE',  ( 0.000000000000000000, -1.000000000000000000, 0.000000000000000000 ) ) ;
#14599 = ORIENTED_EDGE ( 'NONE', *, *, #17364, .T. ) ;
#14600 = AXIS2_PLACEMENT_3D ( 'NONE', #10997, #1791, #20209 ) ;
#14601 = CARTESIAN_POINT ( 'NONE',  ( -15.83717920454666483, 8.841378262663962317, 2.376184731017836782 ) ) ;
#14602 = CARTESIAN_POINT ( 'NONE',  ( -24.59729957373000175, 9.304297380551000529, -4.183949263271999897 ) ) ;
#14603 = CARTESIAN_POINT ( 'NONE',  ( -2.500000000000000000, 29.60000000000000142, 0.000000000000000000 ) ) ;
#14605 = EDGE_CURVE ( 'NONE', #21993, #22807, #5710, .T. ) ;
#14604 = CARTESIAN_POINT ( 'NONE',  ( 18.33699999999999974, -9.141845273363999880, 1.095420050962999850E-14 ) ) ;
#14606 = DIRECTION ( 'NONE',  ( -0.9996708941621513800, 0.02565352539213145919, 0.000000000000000000 ) ) ;
#14607 = CARTESIAN_POINT ( 'NONE',  ( -2.098987933218289914, 27.83721252561470649, 0.5526953750194446568 ) ) ;
#14608 = DIRECTION ( 'NONE',  ( 0.000000000000000000, -1.000000000000000000, 0.000000000000000000 ) ) ;
#14609 = CARTESIAN_POINT ( 'NONE',  ( 0.1386669981692911224, 30.79610789710345742, -2.185737362969716546 ) ) ;
#14610 = ORIENTED_EDGE ( 'NONE', *, *, #17551, .F. ) ;
#14611 = CARTESIAN_POINT ( 'NONE',  ( 0.000000000000000000, 26.20000000000000284, -4.618802153517000519 ) ) ;
#14612 = CARTESIAN_POINT ( 'NONE',  ( -22.26176253788000281, -9.242562415387000740, 0.000000000000000000 ) ) ;
#14613 = CARTESIAN_POINT ( 'NONE',  ( 5.302309017544000191, 13.73032573480000096, -4.450985556070999216 ) ) ;
#14614 = AXIS2_PLACEMENT_3D ( 'NONE', #22983, #10284, #10413 ) ;
#14615 = CARTESIAN_POINT ( 'NONE',  ( 4.000000000000000000, 24.80000000000000426, -2.309401076759000304 ) ) ;
#14616 = CARTESIAN_POINT ( 'NONE',  ( -2.088559871480999419, 26.14437716036000126, -1.279883260171999826 ) ) ;
#14617 = DIRECTION ( 'NONE',  ( -1.000000000000000000, 0.000000000000000000, 0.000000000000000000 ) ) ;
#14618 = EDGE_LOOP ( 'NONE', ( #5829, #18431, #3822 ) ) ;
#14619 = CONICAL_SURFACE ( 'NONE', #15004, 4.309401076758999416, 1.119376321708719590 ) ;
#14620 = CARTESIAN_POINT ( 'NONE',  ( -3.184315894841176053, 11.90921843639853606, -3.629752879533585386 ) ) ;
#14621 = CARTESIAN_POINT ( 'NONE',  ( 0.000000000000000000, -1.550000000000000044, 0.000000000000000000 ) ) ;
#14622 = CARTESIAN_POINT ( 'NONE',  ( -3.999895459877826465, 28.20780860099995024, 1.909390889640791622 ) ) ;
#14623 = ORIENTED_EDGE ( 'NONE', *, *, #6288, .F. ) ;
#14624 = CARTESIAN_POINT ( 'NONE',  ( -2.729128784747790970, 19.00000000000000000, 0.000000000000000000 ) ) ;
#14625 = CARTESIAN_POINT ( 'NONE',  ( -14.25243324638999809, 13.93375672974000068, -0.8660254037843999608 ) ) ;
#14626 = CIRCLE ( 'NONE', #686, 3.000000000000000000 ) ;
#14627 = CARTESIAN_POINT ( 'NONE',  ( 15.28425158531000072, -8.882884205749999040, 4.999858360703999693 ) ) ;
#14628 = CARTESIAN_POINT ( 'NONE',  ( 18.59693257352302354, 10.26249244534900029, 1.842170885552584902 ) ) ;
#14629 = FACE_OUTER_BOUND ( 'NONE', #18903, .T. ) ;
#14630 = CARTESIAN_POINT ( 'NONE',  ( -0.6465006763629999043, 28.70297252654999909, 1.951786927810000183 ) ) ;
#14631 = CARTESIAN_POINT ( 'NONE',  ( 24.25008227645999881, 0.000000000000000000, 0.000000000000000000 ) ) ;
#14632 = CARTESIAN_POINT ( 'NONE',  ( 13.49999999999999645, -9.595521044434660141, 1.928683791516291324 ) ) ;
#14633 = ORIENTED_EDGE ( 'NONE', *, *, #2236, .F. ) ;
#14634 = DIRECTION ( 'NONE',  ( 0.000000000000000000, 0.000000000000000000, 1.000000000000000000 ) ) ;
#14635 = CARTESIAN_POINT ( 'NONE',  ( 20.12460122230999815, 9.191763640279999592, -6.496768647051000656 ) ) ;
#14636 = VECTOR ( 'NONE', #2672, 1000.000000000000000 ) ;
#14637 = LINE ( 'NONE', #19985, #19732 ) ;
#14638 = DIRECTION ( 'NONE',  ( 1.000000000000000000, 0.000000000000000000, 0.000000000000000000 ) ) ;
#14639 = AXIS2_PLACEMENT_3D ( 'NONE', #10268, #16061, #21296 ) ;
#14640 = CARTESIAN_POINT ( 'NONE',  ( 0.000000000000000000, -1.550000000000000044, 0.000000000000000000 ) ) ;
#14641 = TOROIDAL_SURFACE ( 'NONE', #16956, 10.50000000000000000, 0.1000000000000000056 ) ;
#14642 = CARTESIAN_POINT ( 'NONE',  ( -12.24999999999999822, 13.59206128970241778, -6.344557540553090291 ) ) ;
#14643 = CARTESIAN_POINT ( 'NONE',  ( 0.1891046077859345476, 29.19254760244434976, -2.151987026392503832 ) ) ;
#14644 = ORIENTED_CLOSED_SHELL ( 'NONE', *, #8877, .F. );
#14645 = CARTESIAN_POINT ( 'NONE',  ( -24.48285595303000051, -9.947371647070999856, -3.562228079131000147 ) ) ;
#14646 = ORIENTED_EDGE ( 'NONE', *, *, #13824, .F. ) ;
#14647 = LINE ( 'NONE', #8737, #12705 ) ;
#14648 = CONICAL_SURFACE ( 'NONE', #6913, 4.699999872533999756, 0.7853981633972997312 ) ;
#14649 = EDGE_LOOP ( 'NONE', ( #12762, #17277, #352, #9001 ) ) ;
#14650 = CARTESIAN_POINT ( 'NONE',  ( 2.235419194099999896, 24.28959072804000030, -0.7352241695104999586 ) ) ;
#14651 = CARTESIAN_POINT ( 'NONE',  ( 6.379286604629002433, 13.55943310907999688, 1.863575392949001763 ) ) ;
#14652 = CARTESIAN_POINT ( 'NONE',  ( 11.07373617191544923, -0.5001676861130824880, -12.49996440465594993 ) ) ;
#14653 = DIRECTION ( 'NONE',  ( -1.000000000000000000, 0.000000000000000000, 0.000000000000000000 ) ) ;
#14654 = CARTESIAN_POINT ( 'NONE',  ( -4.624999963076000142, 12.99999996307999872, -4.214403009264000636E-08 ) ) ;
#14655 = CARTESIAN_POINT ( 'NONE',  ( 18.38193924931000112, 10.76489784149000251, -0.6396482201651000343 ) ) ;
#14656 = AXIS2_PLACEMENT_3D ( 'NONE', #5220, #20226, #5449 ) ;
#14657 = ORIENTED_EDGE ( 'NONE', *, *, #7332, .F. ) ;
#14658 = CARTESIAN_POINT ( 'NONE',  ( -15.00576253787999903, -9.056359154562001024, 0.000000000000000000 ) ) ;
#14659 = AXIS2_PLACEMENT_3D ( 'NONE', #15365, #22756, #15491 ) ;
#14660 = CARTESIAN_POINT ( 'NONE',  ( 4.000000000000000000, 29.69999999999999929, 2.309401076759000304 ) ) ;
#14661 = DIRECTION ( 'NONE',  ( -0.4247135072049882942, 0.9053278062655749636, 0.000000000000000000 ) ) ;
#14662 = ORIENTED_EDGE ( 'NONE', *, *, #10699, .T. ) ;
#14663 = CARTESIAN_POINT ( 'NONE',  ( -19.36326595524999661, -10.58611661219999966, 1.843048566446000125 ) ) ;
#14664 = CARTESIAN_POINT ( 'NONE',  ( -0.2985486204943000321, 23.87271582673999859, 2.123722402587000069 ) ) ;
#14665 = CARTESIAN_POINT ( 'NONE',  ( 14.76958591329545989, 9.026438462397976537, -5.017364683716268203 ) ) ;
#14666 = AXIS2_PLACEMENT_3D ( 'NONE', #18845, #22593, #18614 ) ;
#14667 = CARTESIAN_POINT ( 'NONE',  ( -10.04281598263999875, 20.50000000000000000, -1.000000000000000000 ) ) ;
#14668 = CARTESIAN_POINT ( 'NONE',  ( 18.82728777423999844, 0.006295662015650000005, 10.66412175315999988 ) ) ;
#14669 = FACE_OUTER_BOUND ( 'NONE', #15134, .T. ) ;
#14670 = CARTESIAN_POINT ( 'NONE',  ( 13.69915933970933963, 8.483254755539659797, -3.069216687506281183 ) ) ;
#14671 = CARTESIAN_POINT ( 'NONE',  ( 4.517650654553999168, 12.53108973233999457, -1.707274550749000364 ) ) ;
#14672 = CONICAL_SURFACE ( 'NONE', #10823, 9.157130689899000586, 0.02565634000431304615 ) ;
#14673 = EDGE_CURVE ( 'NONE', #16342, #9790, #4560, .T. ) ;
#14674 = ORIENTED_EDGE ( 'NONE', *, *, #1569, .T. ) ;
#14675 = CARTESIAN_POINT ( 'NONE',  ( -14.60220935799346265, -1.520255290742261733, -8.953970405129554777 ) ) ;
#14676 = CARTESIAN_POINT ( 'NONE',  ( -14.23150127962423994, -7.645023867421874009, 6.980454963417014547 ) ) ;
#14677 = VECTOR ( 'NONE', #7795, 1000.000000000000000 ) ;
#14678 = VECTOR ( 'NONE', #14606, 1000.000000000000000 ) ;
#14679 = ORIENTED_EDGE ( 'NONE', *, *, #21636, .F. ) ;
#14680 = DIRECTION ( 'NONE',  ( 0.000000000000000000, 1.000000000000000000, 0.000000000000000000 ) ) ;
#14681 = CARTESIAN_POINT ( 'NONE',  ( 11.18574820343480525, -11.70054794218647842, -4.734095432798069325 ) ) ;
#14682 = CARTESIAN_POINT ( 'NONE',  ( 21.49345603379665093, 8.058846013972555511, 4.644683092982796246 ) ) ;
#14683 = CARTESIAN_POINT ( 'NONE',  ( 13.54274790051000110, -0.4384800474203000564, 10.98015942592999927 ) ) ;
#14684 = CARTESIAN_POINT ( 'NONE',  ( 23.99062354302999722, 6.216878364870000340, -12.50000000000000000 ) ) ;
#14685 = CARTESIAN_POINT ( 'NONE',  ( -2.464088664829000130, 26.79256359724000092, 0.1453149127352000025 ) ) ;
#14686 = EDGE_CURVE ( 'NONE', #12867, #21635, #17727, .T. ) ;
#14687 = ORIENTED_EDGE ( 'NONE', *, *, #5997, .F. ) ;
#14688 = CARTESIAN_POINT ( 'NONE',  ( -9.487101138770000830, -6.342674860076999543, -13.83369712466000045 ) ) ;
#14689 = CARTESIAN_POINT ( 'NONE',  ( 13.50000000000000178, 8.918778220045556537, -2.986288483409031524 ) ) ;
#14690 = CARTESIAN_POINT ( 'NONE',  ( 0.8491321808655799552, 28.10222989789001247, -4.128541458486335358 ) ) ;
#14691 = VERTEX_POINT ( 'NONE', #10858 ) ;
#14692 = CARTESIAN_POINT ( 'NONE',  ( 23.76474137987780111, 10.57295235097301145, -0.8683397068570842814 ) ) ;
#14693 = CARTESIAN_POINT ( 'NONE',  ( 24.37713355803436599, 9.330746210554012876, -8.838673490789293652 ) ) ;
#14694 = CARTESIAN_POINT ( 'NONE',  ( 16.18775596657570048, -3.143559382843135630, -9.875345798663321517 ) ) ;
#14695 = CARTESIAN_POINT ( 'NONE',  ( -18.95478082342999926, -4.545484222122999185, -10.15604107551000013 ) ) ;
#14696 = CARTESIAN_POINT ( 'NONE',  ( -1.826717418791999892, 30.92821884477999816, -1.467226286860000117 ) ) ;
#14697 = VECTOR ( 'NONE', #20900, 1000.000000000000000 ) ;
#14698 = CARTESIAN_POINT ( 'NONE',  ( -15.55485259867999837, 4.780789984251000213, 8.479691756156000793 ) ) ;
#14699 = EDGE_CURVE ( 'NONE', #3590, #17463, #11526, .T. ) ;
#14700 = CARTESIAN_POINT ( 'NONE',  ( 1.985433307355395360, 29.85536931078693001, -0.8508083005501347884 ) ) ;
#14701 = ORIENTED_EDGE ( 'NONE', *, *, #19465, .F. ) ;
#14702 = CARTESIAN_POINT ( 'NONE',  ( 0.4793969798898999879, 24.06092953115000199, 2.128160979441000134 ) ) ;
#14703 = CARTESIAN_POINT ( 'NONE',  ( 20.55460958469728538, 8.198441454514611593, 6.607155824187043613 ) ) ;
#14704 = CARTESIAN_POINT ( 'NONE',  ( -14.00000000000000000, -15.45000000000000107, 0.000000000000000000 ) ) ;
#14705 = ORIENTED_EDGE ( 'NONE', *, *, #7744, .T. ) ;
#14706 = DIRECTION ( 'NONE',  ( 0.000000000000000000, 0.000000000000000000, -1.000000000000000000 ) ) ;
#14707 = CARTESIAN_POINT ( 'NONE',  ( 4.834946199837999892, 12.42232141699000181, 0.1060585776307999689 ) ) ;
#14708 = EDGE_LOOP ( 'NONE', ( #7976, #14361, #5626, #22642 ) ) ;
#14709 = EDGE_CURVE ( 'NONE', #10709, #16663, #19708, .T. ) ;
#14710 = CARTESIAN_POINT ( 'NONE',  ( 14.57325125730999993, -2.690795753208000018, 8.752124397991998705 ) ) ;
#14711 = ORIENTED_EDGE ( 'NONE', *, *, #5047, .T. ) ;
#14712 = CARTESIAN_POINT ( 'NONE',  ( -5.057059693511116727, 15.90694920458252071, 3.455692463001508230 ) ) ;
#14713 = DIRECTION ( 'NONE',  ( 0.000000000000000000, 0.000000000000000000, -1.000000000000000000 ) ) ;
#14714 = ORIENTED_EDGE ( 'NONE', *, *, #19314, .F. ) ;
#14715 = CARTESIAN_POINT ( 'NONE',  ( 2.500000000000000000, 24.41665956134495730, -0.3271097220832465124 ) ) ;
#14716 = CARTESIAN_POINT ( 'NONE',  ( -20.31345166415999870, 6.452540530572000499, 8.416401568578999459 ) ) ;
#14717 = CARTESIAN_POINT ( 'NONE',  ( 11.90008533511957367, -8.504566836174662470, -10.26973740115090017 ) ) ;
#14718 = CARTESIAN_POINT ( 'NONE',  ( -5.273521783973994737, 14.65714449329999702, -3.721049535021002441 ) ) ;
#14719 = CARTESIAN_POINT ( 'NONE',  ( -23.36664997781829456, -5.995105419842714944, 8.715914855933332817 ) ) ;
#14720 = CARTESIAN_POINT ( 'NONE',  ( 2.151176768373039838, 27.38669294409674393, 0.3026932924341791398 ) ) ;
#14721 = CARTESIAN_POINT ( 'NONE',  ( 1.399999855176999874, 6.999999855177000185, -5.700011344538000517E-07 ) ) ;
#14722 = CARTESIAN_POINT ( 'NONE',  ( -0.8328668639932000906, 29.02250240009999871, 2.747163055864000114 ) ) ;
#14723 = EDGE_CURVE ( 'NONE', #9190, #1429, #21872, .T. ) ;
#14724 = CARTESIAN_POINT ( 'NONE',  ( 1.949611214030006812, 30.66062952581684087, -0.9304744684606878202 ) ) ;
#14725 = ORIENTED_EDGE ( 'NONE', *, *, #16379, .F. ) ;
#14726 = EDGE_CURVE ( 'NONE', #11568, #10983, #3028, .T. ) ;
#14727 = CARTESIAN_POINT ( 'NONE',  ( -18.99854661335000117, -6.966878364870000340, -12.06698729810999993 ) ) ;
#14728 = CARTESIAN_POINT ( 'NONE',  ( 4.616100662420898004, 13.51152904214929684, -5.077026504744428514 ) ) ;
#14729 = CARTESIAN_POINT ( 'NONE',  ( -24.23230866834131447, 0.5965514821640681697, -10.58710619923159335 ) ) ;
#14730 = CARTESIAN_POINT ( 'NONE',  ( -2.218121370661999769, 28.35614211381999894, -0.5788358281067000899 ) ) ;
#14731 = LINE ( 'NONE', #22799, #20075 ) ;
#14732 = CARTESIAN_POINT ( 'NONE',  ( 4.797639067608940877, 12.42995552893798994, 0.8516731598688934701 ) ) ;
#14733 = EDGE_LOOP ( 'NONE', ( #12712, #17826, #13064, #5225 ) ) ;
#14734 = CARTESIAN_POINT ( 'NONE',  ( -0.6749559008190714193, 11.50211200430284464, -4.764868824692928939 ) ) ;
#14735 = EDGE_CURVE ( 'NONE', #16006, #3092, #19824, .T. ) ;
#14736 = DIRECTION ( 'NONE',  ( 0.9999999999999453770, -3.279696922991151128E-07, -4.019963350050187028E-08 ) ) ;
#14737 = EDGE_CURVE ( 'NONE', #20461, #6021, #3781, .T. ) ;
#14738 = CARTESIAN_POINT ( 'NONE',  ( -3.999987874060712656, 28.10222989788994497, 1.328900689436825377 ) ) ;
#14739 = ORIENTED_EDGE ( 'NONE', *, *, #3061, .F. ) ;
#14740 = LINE ( 'NONE', #7467, #1063 ) ;
#14741 = B_SPLINE_CURVE_WITH_KNOTS ( 'NONE', 3,
 ( #10713, #12645, #23774, #18104, #10945, #23891, #18222, #8901, #17982, #9011, #3213, #5377, #14689, #12418, #1510, #3452, #8651, #10597, #16268, #8777, #23660, #1384, #22081, #16015, #12528, #20154, #1741, #7070, #1623, #16382, #5148, #16138, #23541, #19917, #3332, #5489, #6953, #14570, #14454, #7297, #20034, #16500, #7176, #21848 ),
 .UNSPECIFIED., .F., .F.,
 ( 4, 1, 1, 1, 1, 1, 2, 2, 1, 1, 1, 1, 1, 2, 2, 1, 1, 1, 1, 2, 2, 2, 1, 1, 2, 2, 1, 1, 2, 2, 4 ),
 ( 0.000000000000000000, 0.1249999999999985567, 0.1874999999999978906, 0.2187499999999975575, 0.2343749999999973632, 0.2421874999999973355, 0.2460937499999973355, 0.2499999999999973355, 0.3124999999999971134, 0.3437499999999970024, 0.3593749999999969469, 0.3671874999999969469, 0.3710937499999969469, 0.3730468749999968914, 0.3749999999999968914, 0.4374999999999970579, 0.4687499999999971134, 0.4843749999999971689, 0.4921874999999972244, 0.4960937499999972244, 0.4999999999999972244, 0.6249999999999978906, 0.6874999999999982236, 0.7187499999999984457, 0.7343749999999985567, 0.7499999999999985567, 0.8124999999999988898, 0.8437499999999990008, 0.8593749999999992228, 0.8749999999999993339, 1.000000000000000000 ),
 .UNSPECIFIED. ) ;
#14742 = CARTESIAN_POINT ( 'NONE',  ( 17.58768908531000008, -3.881224882977999613, -9.490963515925001204 ) ) ;
#14743 = CARTESIAN_POINT ( 'NONE',  ( 18.81497143630078384, 6.186105294716906400, 8.399328565840326277 ) ) ;
#14744 = DIRECTION ( 'NONE',  ( -1.000000000000000000, 0.000000000000000000, 0.000000000000000000 ) ) ;
#14745 = CARTESIAN_POINT ( 'NONE',  ( 1.263454500199000075, 30.42364525888999793, 1.740526072561999982 ) ) ;
#14746 = FACE_OUTER_BOUND ( 'NONE', #23481, .T. ) ;
#14747 = CARTESIAN_POINT ( 'NONE',  ( 13.50000000000000178, -7.996356175792731058, 6.080764513117456360 ) ) ;
#14748 = VERTEX_POINT ( 'NONE', #12554 ) ;
#14749 = DIRECTION ( 'NONE',  ( 0.000000000000000000, 1.000000000000000000, 0.000000000000000000 ) ) ;
#14750 = CARTESIAN_POINT ( 'NONE',  ( 21.10410220312999741, -2.836328727688000040, 10.37276910986000011 ) ) ;
#14751 = FACE_OUTER_BOUND ( 'NONE', #7441, .T. ) ;
#14752 = ORIENTED_EDGE ( 'NONE', *, *, #22715, .T. ) ;
#14753 = CARTESIAN_POINT ( 'NONE',  ( -11.04281598264000053, 1.359882291614000008E-14, 0.000000000000000000 ) ) ;
#14754 = CARTESIAN_POINT ( 'NONE',  ( 24.49999999999999645, 4.566319020512484173, 9.204673959736052069 ) ) ;
#14755 = CARTESIAN_POINT ( 'NONE',  ( 4.326177836376999153, 12.22448935855999430, 2.345174457005999802 ) ) ;
#14756 = CARTESIAN_POINT ( 'NONE',  ( 0.3018188377541565215, 29.18586512010584855, -2.138794871149622967 ) ) ;
#14757 = CARTESIAN_POINT ( 'NONE',  ( -20.30574230851999928, 6.911969653458998941, -8.632951638288000495 ) ) ;
#14758 = VERTEX_POINT ( 'NONE', #1535 ) ;
#14759 = ORIENTED_EDGE ( 'NONE', *, *, #5856, .F. ) ;
#14760 = CARTESIAN_POINT ( 'NONE',  ( -0.8914544781580999722, 24.49860156660999877, -2.177834349592000063 ) ) ;
#14761 = CARTESIAN_POINT ( 'NONE',  ( 4.820143762837000523, 14.15667339170999739, 4.018455007228999065 ) ) ;
#14762 = CARTESIAN_POINT ( 'NONE',  ( 11.72559253309821514, -4.116598456382959625, -12.49995860919746171 ) ) ;
#14763 = CARTESIAN_POINT ( 'NONE',  ( -14.00000000000000000, 10.59999999999999964, 0.000000000000000000 ) ) ;
#14764 = DIRECTION ( 'NONE',  ( 0.000000000000000000, 0.000000000000000000, -1.000000000000000000 ) ) ;
#14765 = CARTESIAN_POINT ( 'NONE',  ( 15.28425158531000072, -8.882884205749999040, 4.999858360703999693 ) ) ;
#14766 = CIRCLE ( 'NONE', #14385, 3.850000000000000977 ) ;
#14767 = SHAPE_REPRESENTATION_RELATIONSHIP ( 'NONE' , 'NONE' ,  #12781, #10832 ) ;
#14768 = ORIENTED_EDGE ( 'NONE', *, *, #5954, .F. ) ;
#14769 = CARTESIAN_POINT ( 'NONE',  ( -18.73722805020999616, -7.945584595330000610, 4.815966472443999891 ) ) ;
#14770 = DIRECTION ( 'NONE',  ( -0.9996708941621516020, 0.02565352539211874019, 3.461521573581829412E-14 ) ) ;
#14771 = DIRECTION ( 'NONE',  ( -0.000000000000000000, 1.000000000000000000, 0.000000000000000000 ) ) ;
#14772 = EDGE_LOOP ( 'NONE', ( #23651, #10739, #3795, #14342 ) ) ;
#14773 = CARTESIAN_POINT ( 'NONE',  ( -10.05754950027480810, 16.19676296412049510, -1.000000000000009992 ) ) ;
#14774 = CARTESIAN_POINT ( 'NONE',  ( 2.331686743179000043, 24.79193902659000059, -0.1260324335329000012 ) ) ;
#14775 = CARTESIAN_POINT ( 'NONE',  ( 14.54050418697157632, 2.709612435072900727, -9.959934958062799382 ) ) ;
#14776 = CARTESIAN_POINT ( 'NONE',  ( 3.000000000000000000, 20.00000000000000000, 0.000000000000000000 ) ) ;
#14777 = CARTESIAN_POINT ( 'NONE',  ( 24.01511664711999927, 10.71773449166999903, -3.585769948605999957 ) ) ;
#14778 = CARTESIAN_POINT ( 'NONE',  ( -1.046351349501999817, 29.04353571299000336, -2.115973140337000125 ) ) ;
#14779 = CARTESIAN_POINT ( 'NONE',  ( 13.72233838329553990, 8.705364101347321082, -2.397688811983387680 ) ) ;
#14780 = CARTESIAN_POINT ( 'NONE',  ( 0.3670138381986997600, 11.65918066382002216, -4.834738583209002627 ) ) ;
#14781 = DIRECTION ( 'NONE',  ( 0.000000000000000000, 0.000000000000000000, -1.000000000000000000 ) ) ;
#14782 = CARTESIAN_POINT ( 'NONE',  ( 21.49165366772000141, -3.200527125370999926, -10.97220403775999920 ) ) ;
#14783 = ORIENTED_EDGE ( 'NONE', *, *, #5645, .F. ) ;
#14784 = AXIS2_PLACEMENT_3D ( 'NONE', #14320, #7044, #12265 ) ;
#14785 = CARTESIAN_POINT ( 'NONE',  ( 2.899999999999999911, 19.00000000000000000, 0.000000000000000000 ) ) ;
#14786 = VERTEX_POINT ( 'NONE', #23794 ) ;
#14787 = B_SPLINE_SURFACE_WITH_KNOTS ( 'NONE', 3, 3, ( 
 ( #17797, #8584, #3144, #938, #12100, #14027, #14269, #12218, #19486, #21667, #5079, #19844, #10275, #2893, #15587, #17665, #18031, #19608, #8220, #19962, #7458, #6998, #20431, #16426, #23595, #3605, #23939, #3717, #11107, #14616, #9055, #10988, #3381, #5534, #11236 ),
 ( #18156, #20197, #18265, #22012, #14840, #22125, #12914, #13032, #1559, #5425, #20312, #14387, #18492, #10764, #22232, #16547, #18372, #8944, #1665, #23815, #7223, #1904, #9293, #14500, #16667, #73, #3840, #1434, #12807, #5647, #5304, #21780, #1783, #16312, #8832 ),
 ( #9171, #5193, #7346, #23703, #14730, #16193, #7110, #12574, #21893, #12695, #20084, #3497, #10877, #16777, #22828, #20909, #22708, #13157, #16900, #9408, #9760, #2371, #5772, #4314, #6118, #22354, #543, #3960, #18724, #15442, #20549, #6242, #2134, #5885, #13271 ),
 ( #21021, #17028, #9880, #13385, #20785, #4192, #11353, #186, #426, #11588, #7826, #7578, #18964, #17147, #17269, #20665, #305, #2019, #9523, #13510, #4075, #13625, #7711, #667, #14957, #4434, #9645, #15079, #7948, #15317, #11704, #19078, #15197, #2250, #2491 ) ),
 .UNSPECIFIED., .F., .F., .F.,
 ( 4, 4 ),
 ( 4, 1, 1, 1, 1, 1, 1, 1, 1, 1, 1, 1, 1, 1, 1, 1, 1, 1, 1, 1, 1, 1, 1, 1, 1, 1, 1, 1, 1, 1, 1, 1, 4 ),
 ( -0.2678694646895999898, 1.311704223562000005 ),
 ( -0.02000000000000000042, 0.01250000000000000069, 0.04499999999999999833, 0.07749999999999999944, 0.1100000000000000006, 0.1424999999999999878, 0.1749999999999999889, 0.2074999999999999900, 0.2399999999999999911, 0.2725000000000000200, 0.3049999999999999933, 0.3375000000000000222, 0.3699999999999999956, 0.4025000000000000244, 0.4349999999999999978, 0.4675000000000000266, 0.5000000000000000000, 0.5324999999999999734, 0.5649999999999999467, 0.5975000000000000311, 0.6300000000000000044, 0.6624999999999999778, 0.6949999999999999512, 0.7275000000000000355, 0.7600000000000000089, 0.7924999999999999822, 0.8249999999999999556, 0.8575000000000000400, 0.8900000000000000133, 0.9224999999999999867, 0.9549999999999999600, 0.9875000000000000444, 1.020000000000000018 ),
 .UNSPECIFIED. ) ;
#14788 = DIRECTION ( 'NONE',  ( 0.000000000000000000, -1.000000000000000000, 0.000000000000000000 ) ) ;
#14789 = CARTESIAN_POINT ( 'NONE',  ( 21.87137270046332915, -2.416481638450508118, 8.992294409326092364 ) ) ;
#14790 = CARTESIAN_POINT ( 'NONE',  ( 18.77582393802000382, 7.032165450859999112, 8.630870596427000052 ) ) ;
#14791 = DIRECTION ( 'NONE',  ( -1.000000000000000000, 0.000000000000000000, 0.000000000000000000 ) ) ;
#14792 = CARTESIAN_POINT ( 'NONE',  ( 1.528152797339000113, 26.50006359724000049, -1.938452583514000072 ) ) ;
#14793 = EDGE_LOOP ( 'NONE', ( #11182, #545 ) ) ;
#14794 = CARTESIAN_POINT ( 'NONE',  ( -10.00358756584999931, 4.021542441345999919, 14.31380562870000084 ) ) ;
#14795 = DIRECTION ( 'NONE',  ( -0.8660254037844288266, 0.000000000000000000, 0.5000000000000169864 ) ) ;
#14796 = DIRECTION ( 'NONE',  ( -1.000000000000000000, 0.000000000000000000, 0.000000000000000000 ) ) ;
#14797 = ADVANCED_FACE ( 'NONE', ( #1292 ), #287, .F. ) ;
#14798 = ORIENTED_EDGE ( 'NONE', *, *, #3900, .T. ) ;
#14799 = CARTESIAN_POINT ( 'NONE',  ( -23.74465998031000069, 7.716878364870000340, 11.63397459621999985 ) ) ;
#14800 = CARTESIAN_POINT ( 'NONE',  ( 20.05850351405853260, 9.867115815705442827, -3.636978922065039033 ) ) ;
#14801 = AXIS2_PLACEMENT_3D ( 'NONE', #7627, #3762, #349 ) ;
#14802 = CARTESIAN_POINT ( 'NONE',  ( 24.43449445986659896, 9.725059455069036574, -8.155702917191968382 ) ) ;
#14803 = CARTESIAN_POINT ( 'NONE',  ( 15.93942490395575895, -9.558381615799778075, -3.992934203908755197 ) ) ;
#14804 = CARTESIAN_POINT ( 'NONE',  ( -17.32881098813999898, -9.732670078718998141, -5.300370996713000160 ) ) ;
#14805 = CARTESIAN_POINT ( 'NONE',  ( -0.7087001424027000729, 30.63054677757000022, -2.075015324932000027 ) ) ;
#14806 = CARTESIAN_POINT ( 'NONE',  ( -16.16424364259000157, 4.823843515939000071, -8.474820356344999084 ) ) ;
#14807 = EDGE_CURVE ( 'NONE', #14786, #8812, #16147, .T. ) ;
#14808 = CARTESIAN_POINT ( 'NONE',  ( 1.293847722389922739, 29.92197960974256432, -1.729741070547694104 ) ) ;
#14809 = ORIENTED_EDGE ( 'NONE', *, *, #14594, .F. ) ;
#14810 = CARTESIAN_POINT ( 'NONE',  ( -1.971011845997999945, 24.68910942064999858, 0.9348812773489000305 ) ) ;
#14811 = CARTESIAN_POINT ( 'NONE',  ( 22.56911982475166312, 2.085580828976256740, 10.36943491226754510 ) ) ;
#14812 = CARTESIAN_POINT ( 'NONE',  ( -1.070116364160798250, 23.62009658023850633, -1.830887543399779993 ) ) ;
#14813 = ORIENTED_EDGE ( 'NONE', *, *, #7474, .T. ) ;
#14814 = CARTESIAN_POINT ( 'NONE',  ( 24.36165043081787118, -3.174800876238296876, 12.50000000000000178 ) ) ;
#14815 = CARTESIAN_POINT ( 'NONE',  ( -14.25546138242000005, -6.466299263714999412, -12.35599677691000053 ) ) ;
#14816 = CARTESIAN_POINT ( 'NONE',  ( -14.00000000000000000, -10.29545622790075754, 0.7917248717053737561 ) ) ;
#14817 = CARTESIAN_POINT ( 'NONE',  ( 15.01200125731000057, -8.889299820566000321, -2.243156938537000045 ) ) ;
#14818 = ORIENTED_EDGE ( 'NONE', *, *, #1856, .F. ) ;
#14819 = CYLINDRICAL_SURFACE ( 'NONE', #5210, 4.750000000000000000 ) ;
#14820 = CARTESIAN_POINT ( 'NONE',  ( 0.6543697108982093891, 29.83333333333333570, 2.434931691670787046 ) ) ;
#14821 = EDGE_CURVE ( 'NONE', #14758, #9876, #2228, .T. ) ;
#14822 = ORIENTED_EDGE ( 'NONE', *, *, #2148, .T. ) ;
#14823 = CARTESIAN_POINT ( 'NONE',  ( -15.76159587121333061, 7.930222888495088718, 4.570839928504368821 ) ) ;
#14824 = CARTESIAN_POINT ( 'NONE',  ( -3.922083573187000294, 12.31548052424001760, 2.678017928241000600 ) ) ;
#14825 = CARTESIAN_POINT ( 'NONE',  ( -22.29709339959999781, -5.613794202598000105, 7.812648601633999768 ) ) ;
#14826 = CARTESIAN_POINT ( 'NONE',  ( -14.13625157436999835, 5.599074946036999734, -7.913639695747000324 ) ) ;
#14827 = CARTESIAN_POINT ( 'NONE',  ( 18.97945833333333354, 5.628133138040521288, -7.323704213949056019 ) ) ;
#14828 = CARTESIAN_POINT ( 'NONE',  ( -19.66079187015698437, -8.028560904012943311, 6.742129426872167208 ) ) ;
#14829 = DIRECTION ( 'NONE',  ( 0.000000000000000000, -1.000000000000000000, 0.000000000000000000 ) ) ;
#14830 = DIRECTION ( 'NONE',  ( 0.000000000000000000, 0.000000000000000000, 1.000000000000000000 ) ) ;
#14832 = AXIS2_PLACEMENT_3D ( 'NONE', #11416, #16975, #376 ) ;
#14831 = CARTESIAN_POINT ( 'NONE',  ( 7.500000000000000000, 26.50000000000000000, -6.000000000000000000 ) ) ;
#14833 = EDGE_CURVE ( 'NONE', #1589, #16783, #1474, .T. ) ;
#14834 = CARTESIAN_POINT ( 'NONE',  ( -2.000000000000000000, 30.00000000000000000, 3.464101615137999968 ) ) ;
#14835 = VERTEX_POINT ( 'NONE', #11273 ) ;
#14836 = CARTESIAN_POINT ( 'NONE',  ( -17.84603743917333674, 1.195142481609348328, -9.129246206417464649 ) ) ;
#14837 = CARTESIAN_POINT ( 'NONE',  ( 19.01495727369000122, -0.2433744186648999774, -9.751344288430999541 ) ) ;
#14838 = CARTESIAN_POINT ( 'NONE',  ( 13.56234160357046292, -2.191821534187185172, -8.802344811741308561 ) ) ;
#14839 = CARTESIAN_POINT ( 'NONE',  ( -23.83066304303370941, 10.51063228770324542, -1.301520733571610133 ) ) ;
#14840 = CARTESIAN_POINT ( 'NONE',  ( -2.213655236985999863, 28.60021896306000144, -0.5776703561810999643 ) ) ;
#14841 = AXIS2_PLACEMENT_3D ( 'NONE', #5314, #12468, #3269 ) ;
#14842 = CARTESIAN_POINT ( 'NONE',  ( -2.124682394174019162, 30.86598673310974661, 0.1994363584945500478 ) ) ;
#14843 = B_SPLINE_CURVE_WITH_KNOTS ( 'NONE', 3,
 ( #12008, #12127, #8734, #6662, #8860, #6547, #18058, #10184, #23621, #19637, #2803, #6784, #3171, #6909, #14302, #1219, #12250, #4987 ),
 .UNSPECIFIED., .F., .F.,
 ( 4, 2, 2, 2, 2, 2, 2, 2, 4 ),
 ( 0.000000000000000000, 0.1250000000000000555, 0.2500000000000000555, 0.3750000000000000000, 0.4999999999999999445, 0.6249999999999998890, 0.7500000000000000000, 0.8750000000000000000, 1.000000000000000000 ),
 .UNSPECIFIED. ) ;
#14844 = CARTESIAN_POINT ( 'NONE',  ( 1.027876147065865720, 11.52789889760357056, 4.702132543716095014 ) ) ;
#14845 = VERTEX_POINT ( 'NONE', #11388 ) ;
#14846 = EDGE_CURVE ( 'NONE', #23190, #13740, #17306, .T. ) ;
#14847 = CARTESIAN_POINT ( 'NONE',  ( -4.677864609647151894, 12.38500653705287213, -1.270735910758368448 ) ) ;
#14848 = CARTESIAN_POINT ( 'NONE',  ( 24.37713355803437310, 12.31988888405492411, 3.661326509212557756 ) ) ;
#14849 = CARTESIAN_POINT ( 'NONE',  ( 2.172683023327428575, 29.59140263288345807, 0.6846090325570640678 ) ) ;
#14850 = VERTEX_POINT ( 'NONE', #1199 ) ;
#14851 = ADVANCED_FACE ( 'NONE', ( #3024 ), #21057, .F. ) ;
#14852 = ADVANCED_FACE ( 'NONE', ( #17433, #19495 ), #827, .T. ) ;
#14853 = CARTESIAN_POINT ( 'NONE',  ( -1.767805011140364924, 26.50018596745192312, 1.767686163102024643 ) ) ;
#14854 = CARTESIAN_POINT ( 'NONE',  ( 14.51643908531000093, 10.16840836635999956, -0.3108424006793999994 ) ) ;
#14855 = CARTESIAN_POINT ( 'NONE',  ( 18.39730916115231096, 9.079266745650221182, -5.115270949334341566 ) ) ;
#14856 = CARTESIAN_POINT ( 'NONE',  ( 0.000000000000000000, 22.00000000000000000, 0.000000000000000000 ) ) ;
#14857 = CARTESIAN_POINT ( 'NONE',  ( 1.461167822581999953, 29.73492324375999729, 1.830009909314999961 ) ) ;
#14858 = CARTESIAN_POINT ( 'NONE',  ( 18.10358580085999947, 2.698449212464999913, -11.10147659952999888 ) ) ;
#14859 = CARTESIAN_POINT ( 'NONE',  ( 0.000000000000000000, 30.00000000000000000, 0.000000000000000000 ) ) ;
#14860 = ORIENTED_EDGE ( 'NONE', *, *, #9816, .T. ) ;
#14861 = DIRECTION ( 'NONE',  ( -1.000000000000000000, 0.000000000000000000, 0.000000000000000000 ) ) ;
#14862 = CARTESIAN_POINT ( 'NONE',  ( 21.98934771389999909, 2.052024005812999707, -10.58059816497999961 ) ) ;
#14863 = EDGE_CURVE ( 'NONE', #22092, #14929, #20269, .T. ) ;
#14864 = CARTESIAN_POINT ( 'NONE',  ( 4.000000000000000000, 30.00000000000000000, 0.000000000000000000 ) ) ;
#14865 = VERTEX_POINT ( 'NONE', #19242 ) ;
#14866 = ADVANCED_FACE ( 'NONE', ( #21182 ), #2655, .F. ) ;
#14867 = CARTESIAN_POINT ( 'NONE',  ( 24.50000000000000355, -6.535120425047818316, 8.327193666827611196 ) ) ;
#14868 = CARTESIAN_POINT ( 'NONE',  ( 24.49999999999999645, 3.559007953318558570, 9.649945607071924059 ) ) ;
#14869 = AXIS2_PLACEMENT_3D ( 'NONE', #5352, #14547, #1487 ) ;
#14870 = CARTESIAN_POINT ( 'NONE',  ( -4.833494663361999066, 12.42176095785000456, -0.1505369627506999708 ) ) ;
#14871 = CARTESIAN_POINT ( 'NONE',  ( -0.7579255142056604555, 29.24940332731515014, -2.022519581349923712 ) ) ;
#14872 = CARTESIAN_POINT ( 'NONE',  ( -22.14367231210000142, 6.201338001754999496, -9.216948840397998666 ) ) ;
#14873 = ORIENTED_EDGE ( 'NONE', *, *, #22155, .F. ) ;
#14874 = B_SPLINE_CURVE_WITH_KNOTS ( 'NONE', 3,
 ( #12599, #3405, #3739, #23727, #11254, #10788, #11010, #9430, #7366, #1583 ),
 .UNSPECIFIED., .F., .F.,
 ( 4, 2, 2, 2, 4 ),
 ( 0.000000000000000000, 0.2500000000000000555, 0.5000000000000001110, 0.7500000000000002220, 1.000000000000000000 ),
 .UNSPECIFIED. ) ;
#14875 = DIRECTION ( 'NONE',  ( -0.7071067811867974839, 0.7071067811862974395, 5.435105086405977277E-09 ) ) ;
#14876 = CIRCLE ( 'NONE', #177, 1.500000000000000000 ) ;
#14877 = ORIENTED_EDGE ( 'NONE', *, *, #23927, .F. ) ;
#14878 = CARTESIAN_POINT ( 'NONE',  ( -1.428961511897999914, 23.73222849182999639, -1.869621096888999912 ) ) ;
#14879 = CARTESIAN_POINT ( 'NONE',  ( 6.642147691535001286, 13.49920999050998915, -0.06642214614436001141 ) ) ;
#14880 = CARTESIAN_POINT ( 'NONE',  ( 1.884954223019000175, 28.16549822781000145, -1.259486242684000112 ) ) ;
#14881 = FACE_OUTER_BOUND ( 'NONE', #9579, .T. ) ;
#14882 = CARTESIAN_POINT ( 'NONE',  ( -19.55887123173999953, -9.833822427806001798, 3.504477313184999776 ) ) ;
#14883 = CARTESIAN_POINT ( 'NONE',  ( 0.000000000000000000, 20.10000000000000142, 0.000000000000000000 ) ) ;
#14884 = CARTESIAN_POINT ( 'NONE',  ( -19.04882659540000134, -6.818301851232999589, 6.682161380682999585 ) ) ;
#14885 = CIRCLE ( 'NONE', #4059, 12.50000000000000178 ) ;
#14886 = CARTESIAN_POINT ( 'NONE',  ( 4.000000000000000888, 29.92936170367563520, 1.090349405812182537 ) ) ;
#14887 = PLANE ( 'NONE',  #2801 ) ;
#14888 = ORIENTED_EDGE ( 'NONE', *, *, #3604, .F. ) ;
#14889 = CARTESIAN_POINT ( 'NONE',  ( -11.04281598264000053, 15.31903517202000131, -1.878299281600999793 ) ) ;
#14890 = CARTESIAN_POINT ( 'NONE',  ( -1.962499827145000042, 25.11214459858999959, -1.265401773453000089 ) ) ;
#14891 = CARTESIAN_POINT ( 'NONE',  ( 14.77323574787787486, 9.091559497059186867, -4.898520349509332128 ) ) ;
#14892 = CARTESIAN_POINT ( 'NONE',  ( -18.21805420454666802, -1.196138244234058678, -9.138792889823502463 ) ) ;
#14893 = CARTESIAN_POINT ( 'NONE',  ( 21.44545916559000176, -11.00422963065999937, -2.246136312581000105 ) ) ;
#14894 = CARTESIAN_POINT ( 'NONE',  ( 2.468126052364000067, 29.51257216720999921, -0.6532334635400000034 ) ) ;
#14895 = EDGE_CURVE ( 'NONE', #5364, #2324, #15480, .T. ) ;
#14896 = CARTESIAN_POINT ( 'NONE',  ( 14.23798725250559905, 0.5470205452132217427, 9.070214828626342651 ) ) ;
#14897 = CARTESIAN_POINT ( 'NONE',  ( -0.5877938013789001381, 11.67164471879000764, -4.806037769057001974 ) ) ;
#14898 = CARTESIAN_POINT ( 'NONE',  ( -2.184465970885641983, 26.70086340285666893, 1.259047450927253564 ) ) ;
#14899 = DIRECTION ( 'NONE',  ( 0.000000000000000000, -1.000000000000000000, 0.000000000000000000 ) ) ;
#14900 = CARTESIAN_POINT ( 'NONE',  ( 11.22311500624865666, 9.824279701796063691, -7.983827916320604956 ) ) ;
#14901 = ORIENTED_EDGE ( 'NONE', *, *, #4236, .T. ) ;
#14902 = CARTESIAN_POINT ( 'NONE',  ( -1.486213254096201197, 24.35414964709700669, 2.050825213284277915 ) ) ;
#14903 = CARTESIAN_POINT ( 'NONE',  ( 0.000000000000000000, 19.09999999999999787, 0.000000000000000000 ) ) ;
#14904 = ORIENTED_EDGE ( 'NONE', *, *, #6152, .F. ) ;
#14905 = CARTESIAN_POINT ( 'NONE',  ( 24.36414987671881605, 9.252522660948818256, 8.974160653052738468 ) ) ;
#14906 = CARTESIAN_POINT ( 'NONE',  ( -3.824747491000654698, 28.25094615491947181, -2.410583160005970171 ) ) ;
#14907 = CARTESIAN_POINT ( 'NONE',  ( 14.83973348638000189, 10.43777180253000125, 3.549999712421000098 ) ) ;
#14908 = DIRECTION ( 'NONE',  ( 0.000000000000000000, 0.000000000000000000, 1.000000000000000000 ) ) ;
#14909 = CARTESIAN_POINT ( 'NONE',  ( -0.2419425476019000099, 26.59756359724000063, -2.456483904114000083 ) ) ;
#14910 = EDGE_LOOP ( 'NONE', ( #13358, #18587, #7001, #5133, #5324, #19678, #2925 ) ) ;
#14911 = VERTEX_POINT ( 'NONE', #4843 ) ;
#14912 = CARTESIAN_POINT ( 'NONE',  ( -11.42172863877000033, -11.83666328600000028, 9.565249431252999202 ) ) ;
#14913 = DIRECTION ( 'NONE',  ( 0.000000000000000000, 0.000000000000000000, 1.000000000000000000 ) ) ;
#14914 = DIRECTION ( 'NONE',  ( 0.000000000000000000, -1.000000000000000000, 0.000000000000000000 ) ) ;
#14915 = ORIENTED_EDGE ( 'NONE', *, *, #10462, .F. ) ;
#14916 = CARTESIAN_POINT ( 'NONE',  ( 19.98391666666666211, -7.737224675997203427, 5.060929617072193132 ) ) ;
#14917 = CARTESIAN_POINT ( 'NONE',  ( 20.23499103147737799, 10.17266449058678646, 2.686287595386958493 ) ) ;
#14918 = VECTOR ( 'NONE', #14117, 1000.000000000000114 ) ;
#14919 = CARTESIAN_POINT ( 'NONE',  ( 6.236038179533940351, 13.70719429076894258, 1.534876996671144189 ) ) ;
#14920 = CARTESIAN_POINT ( 'NONE',  ( 16.07974732740592927, -6.562937474929119830, -8.053821228520819275 ) ) ;
#14921 = CARTESIAN_POINT ( 'NONE',  ( -17.83675921509000162, -8.097439812444001461, 7.586755343379000038 ) ) ;
#14922 = CARTESIAN_POINT ( 'NONE',  ( 2.138161440418999693, 28.76018424004000096, 0.4860145525067000039 ) ) ;
#14923 = CARTESIAN_POINT ( 'NONE',  ( -14.41758667332000066, 9.911104062797001291, 4.224474430483999399 ) ) ;
#14924 = CARTESIAN_POINT ( 'NONE',  ( 1.030379110807799314, 29.66722595074598701, 1.898321818861515187 ) ) ;
#14925 = ORIENTED_EDGE ( 'NONE', *, *, #2737, .T. ) ;
#14926 = CARTESIAN_POINT ( 'NONE',  ( 0.4160319935711000450, 24.39157655595000307, -2.298333837344000319 ) ) ;
#14927 = CARTESIAN_POINT ( 'NONE',  ( 20.63972973568440850, 5.922841969177226495, 8.703777380504034156 ) ) ;
#14928 = CARTESIAN_POINT ( 'NONE',  ( -18.02253305375739245, -2.690258673799740041, 10.10105386629687807 ) ) ;
#14929 = VERTEX_POINT ( 'NONE', #23228 ) ;
#14930 = EDGE_CURVE ( 'NONE', #22357, #903, #13050, .T. ) ;
#14931 = CARTESIAN_POINT ( 'NONE',  ( -4.771322057965996954, 13.13584649598000276, 5.062208158195999452 ) ) ;
#14932 = AXIS2_PLACEMENT_3D ( 'NONE', #3278, #17440, #18831 ) ;
#14933 = CARTESIAN_POINT ( 'NONE',  ( 17.84570833333332374, 1.195141376095346430, 9.129237760912879196 ) ) ;
#14934 = CARTESIAN_POINT ( 'NONE',  ( 16.57406392130999961, -0.9113449805282999305, 9.675305505412000073 ) ) ;
#14935 = ORIENTED_EDGE ( 'NONE', *, *, #15284, .T. ) ;
#14936 = CARTESIAN_POINT ( 'NONE',  ( -4.676970228494227833, 15.63772976374162837, 3.955111732555046000 ) ) ;
#14937 = CARTESIAN_POINT ( 'NONE',  ( 2.434931691670791931, 29.96666666666666856, 0.6543697108981911814 ) ) ;
#14938 = ORIENTED_EDGE ( 'NONE', *, *, #17321, .T. ) ;
#14939 = CIRCLE ( 'NONE', #17666, 2.399999999999999911 ) ;
#14940 = CARTESIAN_POINT ( 'NONE',  ( -22.87210175995843642, 9.258583067823760615, -6.329161777784410158E-06 ) ) ;
#14941 = CARTESIAN_POINT ( 'NONE',  ( -4.379988357423000522, 12.47718658113000778, 1.827485537232998336 ) ) ;
#14942 = VECTOR ( 'NONE', #22364, 1000.000000000000000 ) ;
#14943 = CARTESIAN_POINT ( 'NONE',  ( 12.00000000000000178, 0.4474594423088819051, -9.306393149668425124 ) ) ;
#14944 = CARTESIAN_POINT ( 'NONE',  ( 61.60588651278290939, 37.01856778792605240, -6.000000000000000000 ) ) ;
#14945 = CARTESIAN_POINT ( 'NONE',  ( 2.063594504837999888E-14, 28.80370090847999975, 2.160000000000000142 ) ) ;
#14946 = CARTESIAN_POINT ( 'NONE',  ( -19.84093775038680718, -2.572085328615516087, 10.16682444507051919 ) ) ;
#14947 = CARTESIAN_POINT ( 'NONE',  ( -3.145406728938546781, 26.39685207198636618, -2.802800731853388516 ) ) ;
#14948 = AXIS2_PLACEMENT_3D ( 'NONE', #5807, #2055, #18648 ) ;
#14949 = CARTESIAN_POINT ( 'NONE',  ( 2.184465970885644648, 28.70086340285666537, -1.259047450927249345 ) ) ;
#14950 = CARTESIAN_POINT ( 'NONE',  ( -1.536366799937290084, 28.11753006952332967, -1.999167105995447669 ) ) ;
#14951 = CARTESIAN_POINT ( 'NONE',  ( -0.6790912232653096847, 30.36316110238290022, 2.050354341998521512 ) ) ;
#14952 = ORIENTED_EDGE ( 'NONE', *, *, #1252, .F. ) ;
#14953 = CARTESIAN_POINT ( 'NONE',  ( 18.04870260588999997, 2.058813593266999753, 8.790077575217999595 ) ) ;
#14954 = CARTESIAN_POINT ( 'NONE',  ( 14.74456678153594069, -5.921751136246636626, 6.913021773282147286 ) ) ;
#14955 = ADVANCED_FACE ( 'NONE', ( #10167, #2781 ), #12226, .F. ) ;
#14956 = CARTESIAN_POINT ( 'NONE',  ( -23.00059541739830138, -9.779468793944952054, 4.009870837034711144 ) ) ;
#14957 = CARTESIAN_POINT ( 'NONE',  ( 2.440142399906000126, 26.43946440326000058, -0.3375125786566000041 ) ) ;
#14958 = CARTESIAN_POINT ( 'NONE',  ( -2.127018241980240365, 30.86165161360391807, 0.2199161313900584724 ) ) ;
#14959 = VECTOR ( 'NONE', #14736, 1000.000000000000114 ) ;
#14960 = CARTESIAN_POINT ( 'NONE',  ( 2.791333439079350498, 11.81165397714371146, 3.935739769649145181 ) ) ;
#14961 = VERTEX_POINT ( 'NONE', #15596 ) ;
#14962 = CARTESIAN_POINT ( 'NONE',  ( -2.134135751890048560, 11.67542832177916168, -4.323373072577085807 ) ) ;
#14963 = DIRECTION ( 'NONE',  ( 0.000000000000000000, -1.000000000000000000, 0.000000000000000000 ) ) ;
#14964 = AXIS2_PLACEMENT_3D ( 'NONE', #3506, #22022, #15086 ) ;
#14965 = CARTESIAN_POINT ( 'NONE',  ( 4.834778359340923259, 12.44818675736157942, 0.2493437057047861172 ) ) ;
#14966 = VERTEX_POINT ( 'NONE', #13662 ) ;
#14967 = CIRCLE ( 'NONE', #18100, 2.000000000000000000 ) ;
#14968 = EDGE_CURVE ( 'NONE', #21303, #14691, #21584, .T. ) ;
#14969 = LINE ( 'NONE', #16676, #17297 ) ;
#14970 = CARTESIAN_POINT ( 'NONE',  ( 16.05206408531000051, 5.563243567929000655, -8.565419716155998842 ) ) ;
#14971 = CARTESIAN_POINT ( 'NONE',  ( 0.000000000000000000, 13.00000000000000000, -4.625000000000000000 ) ) ;
#14972 = DIRECTION ( 'NONE',  ( 1.000000000000000000, 0.000000000000000000, 0.000000000000000000 ) ) ;
#14973 = CARTESIAN_POINT ( 'NONE',  ( 15.25983580085999947, 2.106191207965000256, 11.14826357266000123 ) ) ;
#14974 = LINE ( 'NONE', #4091, #15067 ) ;
#14975 = TOROIDAL_SURFACE ( 'NONE', #2619, 7.200000000000000178, 0.1000000000000000056 ) ;
#14976 = ORIENTED_EDGE ( 'NONE', *, *, #1934, .F. ) ;
#14977 = EDGE_CURVE ( 'NONE', #7629, #259, #10375, .T. ) ;
#14978 = PLANE ( 'NONE',  #6775 ) ;
#14979 = CARTESIAN_POINT ( 'NONE',  ( 19.94755212015000012, 3.776176937002000411, -10.59849602182999995 ) ) ;
#14980 = PRODUCT_DEFINITION_SHAPE ( 'NONE', 'NONE',  #23972 ) ;
#14981 = CARTESIAN_POINT ( 'NONE',  ( 2.000000000000000000, 30.00000000000000000, 3.464101615137999968 ) ) ;
#14982 = ORIENTED_EDGE ( 'NONE', *, *, #8976, .F. ) ;
#14983 = CARTESIAN_POINT ( 'NONE',  ( 12.24709585780000154, -6.475684366039000217, -6.720579761511999983 ) ) ;
#14984 = CARTESIAN_POINT ( 'NONE',  ( 24.50000000000000000, 7.523013873557660602, 6.698426195502327651 ) ) ;
#14985 = CARTESIAN_POINT ( 'NONE',  ( 4.717414079990003728, 12.37669079585000098, 1.093762868586999559 ) ) ;
#14986 = CARTESIAN_POINT ( 'NONE',  ( -1.632592650705358972, 29.31298059332072370, -1.414061715089352633 ) ) ;
#14987 = EDGE_CURVE ( 'NONE', #5602, #13406, #12108, .T. ) ;
#14988 = CARTESIAN_POINT ( 'NONE',  ( -23.27233823477999763, -8.296294695444000666, 7.433816105003999475 ) ) ;
#14989 = ORIENTED_EDGE ( 'NONE', *, *, #20883, .T. ) ;
#14990 = DIRECTION ( 'NONE',  ( 0.000000000000000000, 0.000000000000000000, -1.000000000000000000 ) ) ;
#14991 = ORIENTED_EDGE ( 'NONE', *, *, #15166, .T. ) ;
#14992 = CARTESIAN_POINT ( 'NONE',  ( 2.158151686652000301, 24.95052917223999955, -0.1158915279824000027 ) ) ;
#14993 = CARTESIAN_POINT ( 'NONE',  ( 5.665862463139001548, 13.86305811703000757, 2.702659249994999069 ) ) ;
#14994 = CARTESIAN_POINT ( 'NONE',  ( 0.1334610483750000021, 27.48299822781000046, -2.263084017374999757 ) ) ;
#14995 = DIRECTION ( 'NONE',  ( 6.465317307631811410E-08, 0.9999999999999703570, 2.351119573244930785E-07 ) ) ;
#14996 = CARTESIAN_POINT ( 'NONE',  ( 0.000000000000000000, 28.00000000000000000, 0.000000000000000000 ) ) ;
#14997 = AXIS2_PLACEMENT_3D ( 'NONE', #22765, #21205, #19640 ) ;
#14998 = CARTESIAN_POINT ( 'NONE',  ( 23.41677564524290744, 34.01856778792605240, -6.000000000000005329 ) ) ;
#14999 = CARTESIAN_POINT ( 'NONE',  ( 13.44600174930999970, -1.304103625722999871, 10.57402029614000050 ) ) ;
#15000 = SHAPE_REPRESENTATION_RELATIONSHIP ( 'NONE' , 'NONE' ,  #8755, #23512 ) ;
#15001 = EDGE_CURVE ( 'NONE', #16783, #8812, #15711, .T. ) ;
#15002 = CARTESIAN_POINT ( 'NONE',  ( -15.18934998397000058, -10.25623436264999988, -0.2727227130009000078 ) ) ;
#15003 = LINE ( 'NONE', #11034, #20999 ) ;
#15004 = AXIS2_PLACEMENT_3D ( 'NONE', #3545, #12628, #18209 ) ;
#15005 = CARTESIAN_POINT ( 'NONE',  ( -14.48875654244860378, -1.295999377397418328, 12.49999522859940448 ) ) ;
#15006 = AXIS2_PLACEMENT_3D ( 'NONE', #18635, #17290, #7849 ) ;
#15007 = ORIENTED_EDGE ( 'NONE', *, *, #5389, .T. ) ;
#15008 = CARTESIAN_POINT ( 'NONE',  ( -19.99161065248000213, 7.877179509649999467, 7.955496492617000648 ) ) ;
#15009 = CARTESIAN_POINT ( 'NONE',  ( -2.292223709382000152, 25.13479219682000121, 1.060295004442999955 ) ) ;
#15010 = CARTESIAN_POINT ( 'NONE',  ( 13.86823306426570745, -9.092836708730331452, 4.860699923063548589 ) ) ;
#15011 = AXIS2_PLACEMENT_3D ( 'NONE', #10998, #7120, #1792 ) ;
#15012 = DIRECTION ( 'NONE',  ( -1.000000000000000000, 0.000000000000000000, 0.000000000000000000 ) ) ;
#15013 = CARTESIAN_POINT ( 'NONE',  ( 0.3501359026391999696, 29.29714551040999737, 2.528984977829000336 ) ) ;
#15014 = CARTESIAN_POINT ( 'NONE',  ( 14.33953349908450647, -2.586167250888467883, 8.677503207046257216 ) ) ;
#15015 = CARTESIAN_POINT ( 'NONE',  ( 16.95684930358444120, 1.053055326748374654, 10.37866837094156658 ) ) ;
#15016 = AXIS2_PLACEMENT_3D ( 'NONE', #7288, #10705, #19910 ) ;
#15017 = ADVANCED_FACE ( 'NONE', ( #6526 ), #8829, .T. ) ;
#15018 = CARTESIAN_POINT ( 'NONE',  ( 11.70388046503181556, 12.85079422502293411, -2.741654745597553955 ) ) ;
#15019 = VERTEX_POINT ( 'NONE', #11586 ) ;
#15020 = ADVANCED_FACE ( 'NONE', ( #2490 ), #13508, .T. ) ;
#15021 = CARTESIAN_POINT ( 'NONE',  ( 1.602306253747700415, 23.96496164759273739, -1.892277031798197395 ) ) ;
#15022 = ORIENTED_EDGE ( 'NONE', *, *, #5689, .T. ) ;
#15023 = CIRCLE ( 'NONE', #22398, 2.899999999999999911 ) ;
#15024 = LINE ( 'NONE', #1729, #12643 ) ;
#15025 = CARTESIAN_POINT ( 'NONE',  ( 24.45564077607145137, 9.795255522623715905, 8.034119761694611839 ) ) ;
#15026 = CARTESIAN_POINT ( 'NONE',  ( 2.500000000000000000, 28.40000000000000213, 0.000000000000000000 ) ) ;
#15027 = AXIS2_PLACEMENT_3D ( 'NONE', #15574, #3005, #15933 ) ;
#15028 = CARTESIAN_POINT ( 'NONE',  ( 15.38108617992000049, -6.523058388743000258, 8.906538625892999050 ) ) ;
#15029 = DIRECTION ( 'NONE',  ( -1.000000000000000000, 0.000000000000000000, 0.000000000000000000 ) ) ;
#15030 = CARTESIAN_POINT ( 'NONE',  ( -2.778011591584000239, 28.14169433609999871, -0.7249434865795999494 ) ) ;
#15031 = EDGE_CURVE ( 'NONE', #8738, #3791, #2247, .T. ) ;
#15032 = ORIENTED_EDGE ( 'NONE', *, *, #10098, .T. ) ;
#15033 = ORIENTED_EDGE ( 'NONE', *, *, #11189, .F. ) ;
#15034 = ADVANCED_FACE ( 'NONE', ( #789 ), #15439, .F. ) ;
#15035 = CARTESIAN_POINT ( 'NONE',  ( -11.61799971169000045, -12.10921122026999974, 9.785496380100999758 ) ) ;
#15036 = CARTESIAN_POINT ( 'NONE',  ( 0.000000000000000000, 28.15000000674550051, -2.249999993254999886 ) ) ;
#15037 = CARTESIAN_POINT ( 'NONE',  ( 17.92512270046333711, 6.868744509127599152, 6.162759146932331511 ) ) ;
#15038 = EDGE_LOOP ( 'NONE', ( #21339, #17615, #17938, #22655 ) ) ;
#15039 = CARTESIAN_POINT ( 'NONE',  ( -14.44600786774907952, 9.403896164508505962, 8.711943152823643288 ) ) ;
#15040 = CARTESIAN_POINT ( 'NONE',  ( 19.23489509943002318, -10.47072900379253468, 0.6798073259081474085 ) ) ;
#15041 = DIRECTION ( 'NONE',  ( 0.7071067811867999264, 0.7071067811862000729, -3.665336548266999286E-07 ) ) ;
#15042 = CARTESIAN_POINT ( 'NONE',  ( 15.58016428004055243, -6.894168022670424278, 7.716933635784287482 ) ) ;
#15043 = CARTESIAN_POINT ( 'NONE',  ( -18.77411750838999893, 2.263382236681999782, -10.88922404772999997 ) ) ;
#15044 = CIRCLE ( 'NONE', #325, 2.270871215252209030 ) ;
#15045 = CARTESIAN_POINT ( 'NONE',  ( 2.061941880494999602, 29.07619810994999909, -0.7328290969762999429 ) ) ;
#15046 = CONICAL_SURFACE ( 'NONE', #18537, 3.049999825846000157, 0.7853981633972997312 ) ;
#15047 = VECTOR ( 'NONE', #10549, 1000.000000000000114 ) ;
#15048 = CARTESIAN_POINT ( 'NONE',  ( -14.21445632535000136, 4.821896674351999756, 9.628268207709998805 ) ) ;
#15049 = CARTESIAN_POINT ( 'NONE',  ( 1.426790630978265417, 29.69555823242072989, 1.621662507842850154 ) ) ;
#15050 = ORIENTED_EDGE ( 'NONE', *, *, #491, .F. ) ;
#15051 = CARTESIAN_POINT ( 'NONE',  ( 1.957984142568000241, 25.87567143413000181, -0.6867741620196999852 ) ) ;
#15052 = CARTESIAN_POINT ( 'NONE',  ( -24.50000000000000000, -5.823431203803898448, -8.822395769081024852 ) ) ;
#15053 = CARTESIAN_POINT ( 'NONE',  ( -18.31192479224129954, 7.074229065390446713, 7.702880875266950866 ) ) ;
#15054 = ORIENTED_EDGE ( 'NONE', *, *, #22236, .F. ) ;
#15055 = CARTESIAN_POINT ( 'NONE',  ( -12.06624327026013077, -13.93375672973986745, 0.000000000000000000 ) ) ;
#15056 = CARTESIAN_POINT ( 'NONE',  ( -5.152812823547000320, 16.37978035709998892, 3.507589799060998548 ) ) ;
#15057 = CARTESIAN_POINT ( 'NONE',  ( -14.00000000000000000, -10.27687089286999900, -0.6428416445564000270 ) ) ;
#15058 = CIRCLE ( 'NONE', #11987, 1.899912543625999373 ) ;
#15059 = CARTESIAN_POINT ( 'NONE',  ( 11.72137625731000021, -1.402369408125999861, -8.972525410429000203 ) ) ;
#15060 = ORIENTED_EDGE ( 'NONE', *, *, #10326, .F. ) ;
#15061 = DIRECTION ( 'NONE',  ( -1.000000000000000000, 0.000000000000000000, 0.000000000000000000 ) ) ;
#15062 = CARTESIAN_POINT ( 'NONE',  ( 1.709999999999999964, 9.000000000000000000, -0.3720215047547999476 ) ) ;
#15063 = ORIENTED_EDGE ( 'NONE', *, *, #10279, .T. ) ;
#15064 = CARTESIAN_POINT ( 'NONE',  ( -0.7783053373570000266, 26.50000000000000000, 5.000000000000000000 ) ) ;
#15065 = CARTESIAN_POINT ( 'NONE',  ( -23.44771454634823726, -3.885502164501489997, -8.583207962873803609 ) ) ;
#15066 = CARTESIAN_POINT ( 'NONE',  ( -4.183799302787003960, 12.40606742070998791, 2.243501369777998189 ) ) ;
#15067 = VECTOR ( 'NONE', #4329, 1000.000000000000000 ) ;
#15068 = CARTESIAN_POINT ( 'NONE',  ( 12.00000000000000000, 3.374757925648287138, -8.478241236122538993 ) ) ;
#15069 = CARTESIAN_POINT ( 'NONE',  ( -14.47793699669672485, 9.918738539663852549, -7.820229401565270244 ) ) ;
#15070 = CARTESIAN_POINT ( 'NONE',  ( -4.901394592536002293, 15.57359934946000379, -3.198976673040998087 ) ) ;
#15071 = CARTESIAN_POINT ( 'NONE',  ( -2.649085689637681096, 26.47444252552742228, -3.089351817498231068 ) ) ;
#15072 = CARTESIAN_POINT ( 'NONE',  ( -1.999167105995453442, 28.15086340285666466, -1.536366799937283645 ) ) ;
#15073 = CARTESIAN_POINT ( 'NONE',  ( 1.735737918923996981, 30.52199503463014452, 1.297044354150451273 ) ) ;
#15074 = ORIENTED_EDGE ( 'NONE', *, *, #20816, .F. ) ;
#15075 = CARTESIAN_POINT ( 'NONE',  ( 23.51229047600000044, 8.801584319611000851, 5.566787828605999522 ) ) ;
#15076 = CARTESIAN_POINT ( 'NONE',  ( 3.192791986568791707, 13.14721640538022918, -5.956854817651988654 ) ) ;
#15077 = CARTESIAN_POINT ( 'NONE',  ( 1.595510613210902484, 29.99040384242091051, 3.697633671484739537 ) ) ;
#15078 = CARTESIAN_POINT ( 'NONE',  ( -21.50111841624438824, -1.002880873098122017, 10.61775532178399395 ) ) ;
#15079 = CARTESIAN_POINT ( 'NONE',  ( -1.368576729846999962, 26.14696440326000015, 2.048219662131999907 ) ) ;
#15080 = CARTESIAN_POINT ( 'NONE',  ( 21.45754691133475944, 36.29044427405463580, -6.000000000000000000 ) ) ;
#15081 = ORIENTED_EDGE ( 'NONE', *, *, #2376, .T. ) ;
#15082 = CARTESIAN_POINT ( 'NONE',  ( -18.29840813844436198, 10.40894792496784937, 1.972660505488252225 ) ) ;
#15083 = DIRECTION ( 'NONE',  ( 0.000000000000000000, 0.000000000000000000, -1.000000000000000000 ) ) ;
#15084 = CARTESIAN_POINT ( 'NONE',  ( 0.000000000000000000, 21.94999982584599962, -3.049999825846000157 ) ) ;
#15085 = CARTESIAN_POINT ( 'NONE',  ( -14.00000000000000000, 8.507292963980999545, 3.029321241734000303 ) ) ;
#15086 = DIRECTION ( 'NONE',  ( 0.8947368421052591669, 0.000000000000000000, 0.4465937565388801156 ) ) ;
#15087 = CARTESIAN_POINT ( 'NONE',  ( 16.92956408530999823, -4.671063266616000575, 9.108730853067999789 ) ) ;
#15088 = EDGE_CURVE ( 'NONE', #16291, #6273, #6798, .T. ) ;
#15089 = CARTESIAN_POINT ( 'NONE',  ( -19.55803988934999893, -9.263500284663999551, 5.614856615822000130 ) ) ;
#15090 = CARTESIAN_POINT ( 'NONE',  ( -19.54076253787999562, 9.172736192578000214, 0.000000000000000000 ) ) ;
#15091 = CARTESIAN_POINT ( 'NONE',  ( 15.93739037305999950, -10.16690263577000053, 3.715714698119999770 ) ) ;
#15092 = CARTESIAN_POINT ( 'NONE',  ( 13.49999999999999822, -8.302679662493304136, -4.371739577444137659 ) ) ;
#15093 = B_SPLINE_CURVE_WITH_KNOTS ( 'NONE', 3,
 ( #17578, #2806, #15739, #8251, #19265, #2680 ),
 .UNSPECIFIED., .F., .F.,
 ( 4, 2, 4 ),
 ( 3.686902641442823701E-05, 0.0005902785358939091793, 0.001143688045373390067 ),
 .UNSPECIFIED. ) ;
#15094 = CARTESIAN_POINT ( 'NONE',  ( -0.3272492347489120990, 28.98333333333332718, 2.500000000000003109 ) ) ;
#15095 = CARTESIAN_POINT ( 'NONE',  ( 25.01064428847000087, 5.914600320551000934, 7.816648658713001296 ) ) ;
#15096 = CARTESIAN_POINT ( 'NONE',  ( 23.99478584076000232, 13.93375672974000068, 0.6736217020456000126 ) ) ;
#15097 = VERTEX_POINT ( 'NONE', #9879 ) ;
#15098 = CARTESIAN_POINT ( 'NONE',  ( 11.47745461310999993, -6.461451563261999986, -6.705806860117999868 ) ) ;
#15099 = CARTESIAN_POINT ( 'NONE',  ( -4.900699999999999612, 1.284663064832999817E-14, 0.000000000000000000 ) ) ;
#15100 = CIRCLE ( 'NONE', #14353, 4.724999999999999645 ) ;
#15101 = CARTESIAN_POINT ( 'NONE',  ( -4.780243194648996941, 12.47971992104001515, 0.1257369525371998809 ) ) ;
#15102 = CARTESIAN_POINT ( 'NONE',  ( 17.71428936713000013, 9.125865291226999076, 0.000000000000000000 ) ) ;
#15103 = EDGE_CURVE ( 'NONE', #20340, #2076, #15312, .T. ) ;
#15104 = CARTESIAN_POINT ( 'NONE',  ( -24.44193005524000029, -0.7742905126174000063, -11.14459677524999925 ) ) ;
#15105 = ORIENTED_EDGE ( 'NONE', *, *, #16296, .T. ) ;
#15106 = CARTESIAN_POINT ( 'NONE',  ( 19.05233531832000082, -1.887707665395999879, 10.26617185442000135 ) ) ;
#15107 = ORIENTED_EDGE ( 'NONE', *, *, #23888, .T. ) ;
#15108 = CARTESIAN_POINT ( 'NONE',  ( -23.74465998031000069, 6.216878364870000340, -12.50000000000000000 ) ) ;
#15109 = CARTESIAN_POINT ( 'NONE',  ( -1.999167105995447224, 28.08333333333333570, 1.536366799937292305 ) ) ;
#15110 = CARTESIAN_POINT ( 'NONE',  ( 1.664720809480999986, 27.38549822781000032, -1.538852087555999892 ) ) ;
#15111 = CARTESIAN_POINT ( 'NONE',  ( 16.65612270046333876, -7.950280935925901460, 4.582400664091437648 ) ) ;
#15112 = CARTESIAN_POINT ( 'NONE',  ( -12.25000000000000000, 6.613190111079999767, -13.46349570337000046 ) ) ;
#15113 = CARTESIAN_POINT ( 'NONE',  ( 0.000000000000000000, 20.00000000000000000, -2.704938617610999654E-14 ) ) ;
#15114 = CARTESIAN_POINT ( 'NONE',  ( -13.36117685223999985, -10.17969989951000009, -0.7718705306884999784 ) ) ;
#15115 = DIRECTION ( 'NONE',  ( 0.000000000000000000, -1.000000000000000000, 0.000000000000000000 ) ) ;
#15116 = CARTESIAN_POINT ( 'NONE',  ( -14.44600785535404164, -2.842816319682948123, 12.49998455206137216 ) ) ;
#15117 = ADVANCED_FACE ( 'NONE', ( #301, #17145 ), #13155, .F. ) ;
#15118 = EDGE_LOOP ( 'NONE', ( #6776, #13557, #1639, #1290 ) ) ;
#15119 = CARTESIAN_POINT ( 'NONE',  ( -2.000000000000000000, 23.00000000000000000, 0.000000000000000000 ) ) ;
#15120 = B_SPLINE_CURVE_WITH_KNOTS ( 'NONE', 3,
 ( #19349, #2628, #15569, #11835, #6130, #2500, #20796, #13884, #11960, #17527, #20919, #679, #2381, #12084, #10022, #2757, #13522, #8085 ),
 .UNSPECIFIED., .F., .F.,
 ( 4, 2, 2, 2, 2, 2, 2, 2, 4 ),
 ( 0.000000000000000000, 0.1250000000000000833, 0.2500000000000001665, 0.3750000000000001665, 0.5000000000000002220, 0.6250000000000002220, 0.7500000000000001110, 0.8750000000000001110, 1.000000000000000000 ),
 .UNSPECIFIED. ) ;
#15121 = ADVANCED_BREP_SHAPE_REPRESENTATION ( '', ( #16648, #4390 ), #17940 ) ;
#15122 = CARTESIAN_POINT ( 'NONE',  ( -2.282676281439000032, 24.90127533745000221, -1.471848595755000044 ) ) ;
#15123 = CARTESIAN_POINT ( 'NONE',  ( 14.36117453097103969, -3.509108449906709115, -9.716323635631455957 ) ) ;
#15124 = LINE ( 'NONE', #11282, #17208 ) ;
#15125 = CARTESIAN_POINT ( 'NONE',  ( 0.5493650718401000832, 28.50724776881999745, 2.493235163772000273 ) ) ;
#15126 = CARTESIAN_POINT ( 'NONE',  ( 11.10357421856130777, 0.9986522863256600546, 12.49997040257240677 ) ) ;
#15127 = CARTESIAN_POINT ( 'NONE',  ( -6.780563428402626158, 15.32813791308405449, -1.804059136873557012 ) ) ;
#15128 = CARTESIAN_POINT ( 'NONE',  ( -6.723317613688290173, 15.34808456536819321, 1.731702247723928112 ) ) ;
#15129 = EDGE_CURVE ( 'NONE', #1991, #8639, #7260, .T. ) ;
#15130 = CARTESIAN_POINT ( 'NONE',  ( 0.000000000000000000, 22.19999999999999574, -4.749999999999798383 ) ) ;
#15131 = ORIENTED_EDGE ( 'NONE', *, *, #5622, .F. ) ;
#15132 = CARTESIAN_POINT ( 'NONE',  ( -14.50606933757998718, 1.515976823860569755, -8.914235622657752600 ) ) ;
#15133 = CARTESIAN_POINT ( 'NONE',  ( -2.818367767609784469, 28.05137445130671381, 2.991616928423204147 ) ) ;
#15134 = EDGE_LOOP ( 'NONE', ( #3300, #16755, #13806, #19873 ) ) ;
#15135 = CARTESIAN_POINT ( 'NONE',  ( -15.99424577250664647, 2.377239741907454906, -8.845303993649501706 ) ) ;
#15136 = VECTOR ( 'NONE', #12133, 1000.000000000000000 ) ;
#15137 = CARTESIAN_POINT ( 'NONE',  ( 24.28455689590255062, 8.829963675777257492, 9.706054284564595847 ) ) ;
#15138 = CARTESIAN_POINT ( 'NONE',  ( 0.000000000000000000, 21.95000012746600149, 0.000000000000000000 ) ) ;
#15139 = ORIENTED_EDGE ( 'NONE', *, *, #20951, .F. ) ;
#15140 = CARTESIAN_POINT ( 'NONE',  ( 15.70815867464999904, -10.50977832323999905, 3.408686822334999533 ) ) ;
#15141 = DIRECTION ( 'NONE',  ( 0.000000000000000000, -1.000000000000000000, 0.000000000000000000 ) ) ;
#15142 = ADVANCED_FACE ( 'NONE', ( #10003 ), #3382, .F. ) ;
#15143 = CARTESIAN_POINT ( 'NONE',  ( -1.483218624018999954, 26.00462896666999768, 2.219793368323999871 ) ) ;
#15144 = ORIENTED_EDGE ( 'NONE', *, *, #6527, .F. ) ;
#15145 = EDGE_LOOP ( 'NONE', ( #11523, #6788, #421, #17150, #15917, #8330, #16457 ) ) ;
#15146 = CARTESIAN_POINT ( 'NONE',  ( -13.99999999999999822, -9.377543214584244780, -3.820245374186972853 ) ) ;
#15147 = AXIS2_PLACEMENT_3D ( 'NONE', #18539, #23515, #14661 ) ;
#15148 = CARTESIAN_POINT ( 'NONE',  ( -11.71982221168999949, -6.976145074222000808, 13.91841713096999911 ) ) ;
#15149 = DIRECTION ( 'NONE',  ( 0.000000000000000000, -1.000000000000000000, 0.000000000000000000 ) ) ;
#15150 = CARTESIAN_POINT ( 'NONE',  ( -12.25000000000000000, -15.45000000000000107, 0.000000000000000000 ) ) ;
#15151 = EDGE_CURVE ( 'NONE', #13107, #5409, #20662, .T. ) ;
#15152 = EDGE_LOOP ( 'NONE', ( #23893, #20604, #3573, #23878 ) ) ;
#15153 = CARTESIAN_POINT ( 'NONE',  ( -19.77404557170999766, 5.276082107202000770, -8.045024713292999508 ) ) ;
#15154 = EDGE_CURVE ( 'NONE', #1842, #6975, #2773, .T. ) ;
#15155 = CARTESIAN_POINT ( 'NONE',  ( 19.78341666666665688, -2.704778927495326002, 8.835500971703069695 ) ) ;
#15156 = CARTESIAN_POINT ( 'NONE',  ( 6.157060429383564681, 14.08832693936469838, 0.3628293340486281604 ) ) ;
#15157 = CARTESIAN_POINT ( 'NONE',  ( 15.67870979658231612, -9.071254133873747350, 4.986216261053892040 ) ) ;
#15158 = CARTESIAN_POINT ( 'NONE',  ( -13.71554468751000044, -9.276193085472000277, -4.453008734943000313 ) ) ;
#15159 = CARTESIAN_POINT ( 'NONE',  ( 0.4716927464761000444, 28.86038704793000065, 2.136794783675000087 ) ) ;
#15160 = CIRCLE ( 'NONE', #18283, 0.09999999999999982514 ) ;
#15161 = CARTESIAN_POINT ( 'NONE',  ( -15.18934998397000058, -10.25623436264999988, -0.2727227130009000078 ) ) ;
#15162 = CARTESIAN_POINT ( 'NONE',  ( 0.3745806831042071683, 29.62585680761208806, 2.127681447449794039 ) ) ;
#15163 = EDGE_CURVE ( 'NONE', #15717, #10339, #18722, .T. ) ;
#15164 = ORIENTED_EDGE ( 'NONE', *, *, #1140, .T. ) ;
#15165 = CARTESIAN_POINT ( 'NONE',  ( -2.173781772047999716, 24.37523480591000080, -0.2297506569266999921 ) ) ;
#15166 = EDGE_CURVE ( 'NONE', #10102, #14442, #21268, .T. ) ;
#15167 = DIRECTION ( 'NONE',  ( 0.000000000000000000, -1.000000000000000000, 0.000000000000000000 ) ) ;
#15168 = CARTESIAN_POINT ( 'NONE',  ( -19.06434331229947077, -2.167475688756183683, -10.25766573832537532 ) ) ;
#15169 = VERTEX_POINT ( 'NONE', #19698 ) ;
#15170 = DIRECTION ( 'NONE',  ( 0.000000000000000000, 1.000000000000000000, 0.000000000000000000 ) ) ;
#15171 = DIRECTION ( 'NONE',  ( 0.000000000000000000, -1.000000000000000000, -2.441144892843000242E-14 ) ) ;
#15172 = DIRECTION ( 'NONE',  ( 0.000000000000000000, -1.000000000000000000, 0.000000000000000000 ) ) ;
#15173 = CARTESIAN_POINT ( 'NONE',  ( 16.46437642130999990, 2.740937500800999960, 9.320585551182000827 ) ) ;
#15174 = ORIENTED_EDGE ( 'NONE', *, *, #18187, .T. ) ;
#15175 = AXIS2_PLACEMENT_3D ( 'NONE', #22653, #19275, #23014 ) ;
#15176 = CARTESIAN_POINT ( 'NONE',  ( -5.951915486294003799, 16.41431975584002245, -1.007191989855000358 ) ) ;
#15177 = CARTESIAN_POINT ( 'NONE',  ( 24.35625626386761056, -12.44383109334005866, 3.446652305529492200 ) ) ;
#15178 = B_SPLINE_SURFACE_WITH_KNOTS ( 'NONE', 3, 3, ( 
 ( #6822, #23536, #17861, #21958, #1620, #8771, #19798, #3207, #6950, #21731, #9121, #5029, #18218, #17977, #21613, #10590, #21844, #21486, #1379, #5371, #5145, #3556, #10941, #12525, #20029, #23657, #10476, #12287, #12760, #8646, #23405, #23770, #8897, #3329, #18328 ),
 ( #14090, #4898, #16265, #7065, #14451, #3448, #5256, #12640, #23285, #19676, #6698, #10833, #3089, #1257, #9008, #16378, #7172, #11178, #9589, #18441, #23884, #15028, #13330, #20264, #14907, #13216, #11533, #7291, #20729, #3788, #4134, #18563, #3667, #20610, #4019 ),
 ( #20501, #2195, #1849, #14790, #9351, #3905, #7656, #2081, #16725, #18912, #22300, #18675, #22426, #18787, #16974, #9471, #375, #11415, #11298, #2320, #15140, #1967, #7773, #22537, #7525, #250, #11055, #135, #5716, #5943, #16494, #13103, #14683, #22076, #5832 ),
 ( #16847, #5484, #24, #5599, #12864, #9238, #16616, #7409, #22185, #12980, #20380, #19272, #7891, #607, #22893, #4628, #17092, #17209, #9944, #4266, #977, #12017, #19143, #6189, #13575, #17330, #2554, #12135, #15383, #19398, #4379, #8009, #20969, #8257, #15260 ) ),
 .UNSPECIFIED., .F., .F., .F.,
 ( 4, 4 ),
 ( 4, 1, 1, 1, 1, 1, 1, 1, 1, 1, 1, 1, 1, 1, 1, 1, 1, 1, 1, 1, 1, 1, 1, 1, 1, 1, 1, 1, 1, 1, 1, 1, 4 ),
 ( -0.6000240009601000013, 1.600024000959999970 ),
 ( -0.01645136390613000099, 0.01028210244132999988, 0.03701556878879000423, 0.06374903513624000095, 0.09048250148370000356, 0.1172159678312000020, 0.1439494341785999831, 0.1706829005261000232, 0.1974163668735000043, 0.2241498332209999889, 0.2508832995683999978, 0.2776167659159000101, 0.3043502322632999912, 0.3310836986108000035, 0.3578171649583000158, 0.3845506313056999970, 0.4112840976532000092, 0.4380175640006000459, 0.4647510303481000027, 0.4914844966954999839, 0.5182179630430000516, 0.5449514293905000084, 0.5716848957378999341, 0.5984183620854000019, 0.6251518284328000385, 0.6518852947802999953, 0.6786187611276999210, 0.7053522274751999888, 0.7320856938227000565, 0.7588191601701000932, 0.7855526265175999390, 0.8122860928649999757, 0.8390195592125000434 ),
 .UNSPECIFIED. ) ;
#15179 = EDGE_LOOP ( 'NONE', ( #335, #12826, #18535, #7269, #5135, #5107 ) ) ;
#15180 = CARTESIAN_POINT ( 'NONE',  ( -6.838539683285000059, 15.31903379280000088, 1.878299112549000061 ) ) ;
#15181 = DIRECTION ( 'NONE',  ( -1.000000000000000000, 0.000000000000000000, 0.000000000000000000 ) ) ;
#15182 = CARTESIAN_POINT ( 'NONE',  ( 3.683742661130003704, 12.24911308434999313, 3.113368964028000896 ) ) ;
#15183 = CARTESIAN_POINT ( 'NONE',  ( 3.999999999999999112, 26.49040384242090695, 0.4670641126941216248 ) ) ;
#15184 = CARTESIAN_POINT ( 'NONE',  ( 12.00000000000000355, 3.681377102019148584, -8.330751794720166359 ) ) ;
#15185 = DIRECTION ( 'NONE',  ( 0.000000000000000000, 1.000000000000000000, 0.000000000000000000 ) ) ;
#15186 = CARTESIAN_POINT ( 'NONE',  ( -3.634800904028002932, 14.60524886664999045, -4.947590794463004649 ) ) ;
#15187 = CARTESIAN_POINT ( 'NONE',  ( -3.268181200173221335, 26.37490599056235752, -2.731916857836431678 ) ) ;
#15188 = CARTESIAN_POINT ( 'NONE',  ( 5.287285710763609536, 13.80050360415835264, -4.264351677957034958 ) ) ;
#15189 = CARTESIAN_POINT ( 'NONE',  ( -2.434931691670790155, 28.20086340285666893, -0.6543697108981963995 ) ) ;
#15190 = CARTESIAN_POINT ( 'NONE',  ( 0.9202813454773431934, 30.45996977815284978, 1.954029222696366030 ) ) ;
#15191 = ORIENTED_EDGE ( 'NONE', *, *, #20206, .T. ) ;
#15192 = CARTESIAN_POINT ( 'NONE',  ( -18.03499577250666164, -4.599986451907970952, -7.981296679855804044 ) ) ;
#15193 = CARTESIAN_POINT ( 'NONE',  ( 22.49347407775999841, -5.087491083399999781, -8.435107541370999940 ) ) ;
#15194 = CARTESIAN_POINT ( 'NONE',  ( -0.06326846155994279852, 12.80354232408877380, -6.663658787853194099 ) ) ;
#15195 = CARTESIAN_POINT ( 'NONE',  ( -23.68078907432000335, -9.459496811531000304, -9.754788243598999975E-09 ) ) ;
#15196 = CARTESIAN_POINT ( 'NONE',  ( -22.14375141673819414, 9.048573216601598190, -5.684411342799975841 ) ) ;
#15197 = CARTESIAN_POINT ( 'NONE',  ( 2.357055497444999759, 25.65946440325999944, -0.7145966149424999303 ) ) ;
#15198 = CIRCLE ( 'NONE', #18322, 2.399999999999999911 ) ;
#15199 = CARTESIAN_POINT ( 'NONE',  ( 12.50897733419000168, -6.466910458125999739, 12.35564390364999987 ) ) ;
#15200 = ORIENTED_EDGE ( 'NONE', *, *, #16612, .T. ) ;
#15201 = CARTESIAN_POINT ( 'NONE',  ( -19.07992278086221205, -8.501993143676337183, -6.120330979234422486 ) ) ;
#15202 = CARTESIAN_POINT ( 'NONE',  ( -2.000000000000000000, 30.00000000000000000, 3.464101615137999968 ) ) ;
#15203 = CARTESIAN_POINT ( 'NONE',  ( -2.147341988817836445, 28.45716134483373594, 0.4763078141162557788 ) ) ;
#15204 = DIRECTION ( 'NONE',  ( -1.000000000000000000, 0.000000000000000000, 0.000000000000000000 ) ) ;
#15205 = ORIENTED_EDGE ( 'NONE', *, *, #9772, .F. ) ;
#15206 = CARTESIAN_POINT ( 'NONE',  ( 4.000000000000000888, 30.00000000000001066, -0.3708744353061897425 ) ) ;
#15207 = CARTESIAN_POINT ( 'NONE',  ( 14.21381424931000126, -3.754242569768000415, -9.992333729823998922 ) ) ;
#15208 = CARTESIAN_POINT ( 'NONE',  ( -15.56314304594000042, -8.450047992442000222, -7.564511025612000061 ) ) ;
#15209 = CARTESIAN_POINT ( 'NONE',  ( -10.04701370329000021, 16.31160201364000173, 0.9999999999983000265 ) ) ;
#15210 = CARTESIAN_POINT ( 'NONE',  ( 14.85358580085999947, 11.33114005906999999, -0.2613888308919999903 ) ) ;
#15211 = LINE ( 'NONE', #7963, #3499 ) ;
#15212 = FACE_OUTER_BOUND ( 'NONE', #10325, .T. ) ;
#15213 = CARTESIAN_POINT ( 'NONE',  ( 25.30572612538999877, -3.463782304174999993, 8.743710282844000758 ) ) ;
#15214 = CARTESIAN_POINT ( 'NONE',  ( 3.560623727957783924, 29.81534065533141131, 2.563075085697513078 ) ) ;
#15215 = VERTEX_POINT ( 'NONE', #3232 ) ;
#15216 = FACE_OUTER_BOUND ( 'NONE', #5737, .T. ) ;
#15217 = CARTESIAN_POINT ( 'NONE',  ( -2.276308483783000103, 26.28456776952000240, -1.394936847711000016 ) ) ;
#15218 = CARTESIAN_POINT ( 'NONE',  ( 4.837505978036000798, 12.42333062333001514, -0.02305947804070000370 ) ) ;
#15219 = CARTESIAN_POINT ( 'NONE',  ( 11.00000000000000000, 10.59999999999999964, 0.000000000000000000 ) ) ;
#15220 = CARTESIAN_POINT ( 'NONE',  ( -22.60400005165999815, 0.1503115455820999702, -11.12042372740999951 ) ) ;
#15221 = ORIENTED_EDGE ( 'NONE', *, *, #9318, .F. ) ;
#15222 = CARTESIAN_POINT ( 'NONE',  ( -1.488573664845307620, 23.70893436307923707, 1.654057013544842025 ) ) ;
#15223 = ORIENTED_EDGE ( 'NONE', *, *, #5008, .T. ) ;
#15224 = EDGE_CURVE ( 'NONE', #18376, #9517, #13791, .T. ) ;
#15225 = CARTESIAN_POINT ( 'NONE',  ( -24.16119556694614090, 4.108075931972949846, -12.49973851150938309 ) ) ;
#15226 = CARTESIAN_POINT ( 'NONE',  ( 8.196152422706999729, 26.90192378864669820, 6.000000000000000000 ) ) ;
#15227 = CARTESIAN_POINT ( 'NONE',  ( 0.000000000000000000, 30.00000000000000000, 0.000000000000000000 ) ) ;
#15228 = CARTESIAN_POINT ( 'NONE',  ( 16.20262270046332631, 4.576539695569029398, 7.940112068752367414 ) ) ;
#15229 = DIRECTION ( 'NONE',  ( 1.000000000000000000, 0.000000000000000000, 0.000000000000000000 ) ) ;
#15230 = CARTESIAN_POINT ( 'NONE',  ( 13.88475174931000033, -10.63832449705000016, -0.7632376485559000390 ) ) ;
#15231 = VECTOR ( 'NONE', #797, 1000.000000000000227 ) ;
#15232 = CARTESIAN_POINT ( 'NONE',  ( -14.57995894006000093, 5.497579849475999758, -8.642519878353001062 ) ) ;
#15233 = CARTESIAN_POINT ( 'NONE',  ( 14.57325125730999993, -2.690795753208000018, 8.752124397991998705 ) ) ;
#15234 = CARTESIAN_POINT ( 'NONE',  ( -14.32799115069592588, 5.161629268601040543, 12.49976764739585455 ) ) ;
#15235 = VERTEX_POINT ( 'NONE', #11948 ) ;
#15236 = EDGE_CURVE ( 'NONE', #20281, #1220, #16881, .T. ) ;
#15237 = CARTESIAN_POINT ( 'NONE',  ( -4.000000000000000000, 29.74995697614769341, 2.103311180602513542 ) ) ;
#15238 = CARTESIAN_POINT ( 'NONE',  ( -2.122588054292000148, 25.00670996802000090, -1.368625184603999845 ) ) ;
#15239 = CARTESIAN_POINT ( 'NONE',  ( 14.26932110114051966, -6.379006366603656275, -8.140519857586468788 ) ) ;
#15240 = CONICAL_SURFACE ( 'NONE', #9079, 9.787173237795000702, 0.7982263333994560339 ) ;
#15241 = VERTEX_POINT ( 'NONE', #17883 ) ;
#15242 = CARTESIAN_POINT ( 'NONE',  ( 3.182410876788997367, 13.14747453192001103, -5.653946747832996778 ) ) ;
#15243 = CARTESIAN_POINT ( 'NONE',  ( -2.717871120395999984, 30.55607970622999758, -0.3891938976568000697 ) ) ;
#15244 = CARTESIAN_POINT ( 'NONE',  ( 12.06371966926070805, 5.117452910143472700, 12.50009924165165742 ) ) ;
#15245 = CARTESIAN_POINT ( 'NONE',  ( 18.37858639674107408, 10.40198410867141376, 1.159838069824709939 ) ) ;
#15246 = FACE_OUTER_BOUND ( 'NONE', #19709, .T. ) ;
#15247 = VECTOR ( 'NONE', #12748, 1000.000000000000000 ) ;
#15248 = CARTESIAN_POINT ( 'NONE',  ( -4.649999849441000421, 14.99999984944626696, 6.648422602291999773E-08 ) ) ;
#15249 = LINE ( 'NONE', #4256, #6931 ) ;
#15250 = VERTEX_POINT ( 'NONE', #23193 ) ;
#15251 = CARTESIAN_POINT ( 'NONE',  ( 0.000000000000000000, 29.69999999999999929, -4.618802153517000519 ) ) ;
#15252 = ORIENTED_EDGE ( 'NONE', *, *, #1410, .T. ) ;
#15253 = EDGE_CURVE ( 'NONE', #17, #14047, #14562, .T. ) ;
#15254 = CARTESIAN_POINT ( 'NONE',  ( -5.735278047652040634, 16.24235446318282072, -2.150590259619544753 ) ) ;
#15256 = CARTESIAN_POINT ( 'NONE',  ( -0.7385364242858543093, 24.44737158853346770, -2.065887602175232818 ) ) ;
#15255 = CYLINDRICAL_SURFACE ( 'NONE', #4622, 4.750000000000000000 ) ;
#15257 = CARTESIAN_POINT ( 'NONE',  ( -6.250000000000000000, 15.73203524433000311, -1.185075242810999852 ) ) ;
#15258 = ORIENTED_EDGE ( 'NONE', *, *, #3156, .F. ) ;
#15259 = VECTOR ( 'NONE', #7756, 1000.000000000000227 ) ;
#15260 = CARTESIAN_POINT ( 'NONE',  ( 13.50891859955000029, 5.685114405159000128, 8.584150509224999226 ) ) ;
#15261 = PLANE ( 'NONE',  #23347 ) ;
#15262 = CARTESIAN_POINT ( 'NONE',  ( 0.000000000000000000, 26.35000000000000142, 0.000000000000000000 ) ) ;
#15263 = VERTEX_POINT ( 'NONE', #23062 ) ;
#15264 = ORIENTED_EDGE ( 'NONE', *, *, #1069, .T. ) ;
#15265 = CARTESIAN_POINT ( 'NONE',  ( -14.00000000000000178, 5.758787634741540096, -7.178423725779616404 ) ) ;
#15266 = CARTESIAN_POINT ( 'NONE',  ( -11.41435471169000060, -15.33547020656999926, -2.685570560817000185 ) ) ;
#15267 = CARTESIAN_POINT ( 'NONE',  ( 0.07252675453223388080, 6.777045746367004853, -1.752615158248006511 ) ) ;
#15268 = DIRECTION ( 'NONE',  ( -0.7071067811881966980, 0.7071067811848966711, -4.825991045650978446E-08 ) ) ;
#15269 = ORIENTED_EDGE ( 'NONE', *, *, #6886, .F. ) ;
#15270 = ADVANCED_FACE ( 'NONE', ( #15673 ), #6845, .T. ) ;
#15271 = CARTESIAN_POINT ( 'NONE',  ( -22.75980177062999843, -4.975256557067000429, 8.932912903997999976 ) ) ;
#15272 = CARTESIAN_POINT ( 'NONE',  ( -14.42499013958002507, 12.50426282926201793, 3.341925919227497488 ) ) ;
#15273 = CARTESIAN_POINT ( 'NONE',  ( 6.191435500673191150, 13.91538564218064522, 0.8033750926635572220 ) ) ;
#15274 = CARTESIAN_POINT ( 'NONE',  ( 15.75535489895502828, -10.05762403353078405, 2.456177552663034280 ) ) ;
#15275 = CARTESIAN_POINT ( 'NONE',  ( -19.24802401720000233, -4.548766302313999255, -10.16337245253999910 ) ) ;
#15276 = CARTESIAN_POINT ( 'NONE',  ( -0.8486101488374000468, 29.83923955014999763, -2.021840421918000175 ) ) ;
#15277 = CARTESIAN_POINT ( 'NONE',  ( -17.70843032205999990, -8.525337246235000777, 7.569901604118999927 ) ) ;
#15278 = EDGE_CURVE ( 'NONE', #12276, #16405, #14939, .T. ) ;
#15279 = CARTESIAN_POINT ( 'NONE',  ( 0.9172437346412692927, 29.65973296616930810, 1.957376652516603421 ) ) ;
#15280 = VERTEX_POINT ( 'NONE', #14238 ) ;
#15281 = CARTESIAN_POINT ( 'NONE',  ( 1.912038027982999822, 24.72422363341000207, 1.059350336922000091 ) ) ;
#15282 = CARTESIAN_POINT ( 'NONE',  ( -18.97752579075431356, 0.9511254547103566992, -10.58491024144955794 ) ) ;
#15283 = ORIENTED_EDGE ( 'NONE', *, *, #8833, .T. ) ;
#15284 = EDGE_CURVE ( 'NONE', #9790, #17141, #19576, .T. ) ;
#15285 = CARTESIAN_POINT ( 'NONE',  ( -4.015026692432003053, 15.25594080015998344, 4.668998453457999354 ) ) ;
#15286 = EDGE_CURVE ( 'NONE', #18824, #16291, #4522, .T. ) ;
#15287 = CARTESIAN_POINT ( 'NONE',  ( -13.99999999999999822, -9.925668012745248348, 2.740213007417764413 ) ) ;
#15288 = AXIS2_PLACEMENT_3D ( 'NONE', #10203, #10330, #16249 ) ;
#15289 = CARTESIAN_POINT ( 'NONE',  ( 12.40593892130999976, 9.405156509668998410, -1.966610333673999955 ) ) ;
#15290 = ORIENTED_EDGE ( 'NONE', *, *, #15630, .F. ) ;
#15291 = VECTOR ( 'NONE', #9433, 1000.000000000000000 ) ;
#15292 = CARTESIAN_POINT ( 'NONE',  ( -6.335698864392003138, 16.42991352047999243, -1.007191989855000358 ) ) ;
#15293 = CARTESIAN_POINT ( 'NONE',  ( 23.99478584078000054, 7.550251870568999379, 11.73017644755000077 ) ) ;
#15294 = VERTEX_POINT ( 'NONE', #21387 ) ;
#15295 = EDGE_CURVE ( 'NONE', #14273, #8084, #9547, .T. ) ;
#15296 = DIRECTION ( 'NONE',  ( 0.000000000000000000, -6.254561278618000321E-11, -1.000000000000000000 ) ) ;
#15297 = CARTESIAN_POINT ( 'NONE',  ( 12.04708237232646262, 8.300001991022620373, 10.62407327353252917 ) ) ;
#15298 = CARTESIAN_POINT ( 'NONE',  ( 4.724321909639998651, 12.53663613935000853, -0.02272734326504999985 ) ) ;
#15299 = CARTESIAN_POINT ( 'NONE',  ( 4.000000000000000000, 26.50000000000000355, 0.000000000000000000 ) ) ;
#15300 = CARTESIAN_POINT ( 'NONE',  ( 18.32366523450733808, 7.502789789981919810, -7.229229197467324397 ) ) ;
#15301 = CARTESIAN_POINT ( 'NONE',  ( 11.99999999999999822, 0.3765524563881427200, -9.313981971731278620 ) ) ;
#15302 = CARTESIAN_POINT ( 'NONE',  ( 19.52828936713000019, 9.172416106433001204, 0.000000000000000000 ) ) ;
#15303 = DIRECTION ( 'NONE',  ( 1.000000000000000000, -5.653314293126999632E-09, 4.083276933743999944E-09 ) ) ;
#15304 = DIRECTION ( 'NONE',  ( 1.000000000000000000, 0.000000000000000000, 0.000000000000000000 ) ) ;
#15305 = CARTESIAN_POINT ( 'NONE',  ( 0.4393762720424915225, 26.31534065533142552, -4.365128144578328317 ) ) ;
#15306 = DIRECTION ( 'NONE',  ( 1.000000000000000000, 0.000000000000000000, 0.000000000000000000 ) ) ;
#15307 = CARTESIAN_POINT ( 'NONE',  ( 0.04514251421120654695, 30.40639362649127975, 2.160055992278567150 ) ) ;
#15308 = ORIENTED_EDGE ( 'NONE', *, *, #4252, .T. ) ;
#15309 = CARTESIAN_POINT ( 'NONE',  ( 21.52721940996000072, 6.681649352278999920, 7.201632472380000038 ) ) ;
#15310 = CARTESIAN_POINT ( 'NONE',  ( 2.441032952700726177, 13.00514025596468670, -6.261105887786398760 ) ) ;
#15311 = CIRCLE ( 'NONE', #8371, 2.750000000000000000 ) ;
#15312 = LINE ( 'NONE', #17026, #4169 ) ;
#15313 = B_SPLINE_CURVE_WITH_KNOTS ( 'NONE', 3,
 ( #4717, #10278, #20528, #16315, #20408 ),
 .UNSPECIFIED., .F., .F.,
 ( 4, 1, 4 ),
 ( 0.000000000000000000, 0.3333333333333000081, 0.4999999972379591262 ),
 .UNSPECIFIED. ) ;
#15314 = VECTOR ( 'NONE', #10542, 1000.000000000000114 ) ;
#15315 = EDGE_CURVE ( 'NONE', #5021, #14322, #8263, .T. ) ;
#15316 = CARTESIAN_POINT ( 'NONE',  ( 1.716841021922666632, 23.94065246303359729, 1.459342451765975879 ) ) ;
#15317 = CARTESIAN_POINT ( 'NONE',  ( -2.100366574696000299, 25.95196440325999987, -1.287118485749000119 ) ) ;
#15318 = ADVANCED_FACE ( 'NONE', ( #14471 ), #8788, .F. ) ;
#15319 = CARTESIAN_POINT ( 'NONE',  ( -6.046589298277226909, 26.49999999999999645, 1.190688249984996006 ) ) ;
#15320 = EDGE_LOOP ( 'NONE', ( #15615, #19934, #11762, #2774, #14714, #11051 ) ) ;
#15321 = CARTESIAN_POINT ( 'NONE',  ( -4.850000000102999920, 12.44999864901999942, -1.732907964652000048E-09 ) ) ;
#15322 = CARTESIAN_POINT ( 'NONE',  ( 23.99062354302999722, -7.716878364870000340, 11.63397459621999985 ) ) ;
#15323 = VECTOR ( 'NONE', #11702, 1000.000000000000000 ) ;
#15324 = CARTESIAN_POINT ( 'NONE',  ( -0.6458848329242314890, 27.79145980994124088, 2.105047925194707403 ) ) ;
#15325 = ORIENTED_EDGE ( 'NONE', *, *, #6857, .T. ) ;
#15326 = ORIENTED_EDGE ( 'NONE', *, *, #2144, .F. ) ;
#15327 = EDGE_CURVE ( 'NONE', #10853, #23711, #16909, .T. ) ;
#15328 = CARTESIAN_POINT ( 'NONE',  ( -18.73259798496000172, -8.620928137991000995, 3.072238420002000314 ) ) ;
#15329 = EDGE_CURVE ( 'NONE', #3196, #23059, #5620, .T. ) ;
#15330 = CIRCLE ( 'NONE', #21939, 2.729128784747790970 ) ;
#15331 = CARTESIAN_POINT ( 'NONE',  ( 13.44600174930999970, -1.304103625722999871, 10.57402029614000050 ) ) ;
#15332 = CARTESIAN_POINT ( 'NONE',  ( -13.53183956624999951, -0.9914182199946000029, -11.24149240260000049 ) ) ;
#15333 = DIRECTION ( 'NONE',  ( 0.000000000000000000, 1.000000000000000000, 0.000000000000000000 ) ) ;
#15334 = CARTESIAN_POINT ( 'NONE',  ( 19.45869494525999954, 0.9204530265265999933, 10.34116613746999924 ) ) ;
#15335 = CARTESIAN_POINT ( 'NONE',  ( -1.095323197919201519, 30.85834471387956413, -1.858592797474962754 ) ) ;
#15336 = CARTESIAN_POINT ( 'NONE',  ( 2.500000000000000000, 27.03419673618999752, 0.000000000000000000 ) ) ;
#15337 = CARTESIAN_POINT ( 'NONE',  ( 21.55245587747999991, -7.890825992760999164, 6.521045315185999947 ) ) ;
#15338 = CARTESIAN_POINT ( 'NONE',  ( 11.01624327026000039, -12.44999999999999929, 0.000000000000000000 ) ) ;
#15339 = EDGE_LOOP ( 'NONE', ( #22385, #5343, #9072, #17479 ) ) ;
#15340 = DIRECTION ( 'NONE',  ( -6.791358400560965595E-08, 0.9999999999999975575, 5.471897964325976456E-09 ) ) ;
#15341 = CARTESIAN_POINT ( 'NONE',  ( 2.322750540216000026, 26.78000240009999899, 1.687576972922000040 ) ) ;
#15342 = AXIS2_PLACEMENT_3D ( 'NONE', #21425, #8225, #15952 ) ;
#15343 = CARTESIAN_POINT ( 'NONE',  ( 4.776862951938002588, 12.47838658620001162, -0.1510428563734999008 ) ) ;
#15344 = CARTESIAN_POINT ( 'NONE',  ( 2.069432874219926166, 29.04090307382888625, -0.6216230384549564780 ) ) ;
#15345 = CARTESIAN_POINT ( 'NONE',  ( -21.62195572587000214, 2.576950381532999934, 10.79137310468999900 ) ) ;
#15346 = ORIENTED_EDGE ( 'NONE', *, *, #820, .F. ) ;
#15347 = AXIS2_PLACEMENT_3D ( 'NONE', #6342, #8289, #21252 ) ;
#15348 = DIRECTION ( 'NONE',  ( 0.000000000000000000, 1.000000000000000000, 0.000000000000000000 ) ) ;
#15349 = ORIENTED_EDGE ( 'NONE', *, *, #10633, .T. ) ;
#15350 = DIRECTION ( 'NONE',  ( 0.000000000000000000, 1.000000000000000000, 0.000000000000000000 ) ) ;
#15351 = CARTESIAN_POINT ( 'NONE',  ( -3.792323924634558363, 12.19803457140297098, 2.925688007707359262 ) ) ;
#15352 = LINE ( 'NONE', #4107, #13034 ) ;
#15353 = B_SPLINE_CURVE_WITH_KNOTS ( 'NONE', 3,
 ( #487, #20852, #9470, #16846, #16724, #20727, #15382, #249 ),
 .UNSPECIFIED., .F., .F.,
 ( 4, 2, 2, 4 ),
 ( 1.477043467946315188E-05, 0.0004760515949908603051, 0.0009373327553022574006, 0.001859895075925053001 ),
 .UNSPECIFIED. ) ;
#15354 = CARTESIAN_POINT ( 'NONE',  ( 0.3169597565512499160, 6.785101045795855157, 1.721165433949310763 ) ) ;
#15355 = CARTESIAN_POINT ( 'NONE',  ( 16.73662674931000183, 9.294473935295998857, 5.382749556855999984 ) ) ;
#15356 = CARTESIAN_POINT ( 'NONE',  ( -18.27706328473999875, 10.02730951802000092, -4.225925492466999778 ) ) ;
#15357 = CARTESIAN_POINT ( 'NONE',  ( 13.47637625730999922, -3.210294990792000203, -8.544406387913998202 ) ) ;
#15358 = CARTESIAN_POINT ( 'NONE',  ( 24.28455689590275668, 12.82067141883539918, -2.793945715430803389 ) ) ;
#15359 = ORIENTED_EDGE ( 'NONE', *, *, #8989, .T. ) ;
#15360 = CARTESIAN_POINT ( 'NONE',  ( 2.147930124081999903, 30.14433166633000027, -1.675020066154000231 ) ) ;
#15361 = CARTESIAN_POINT ( 'NONE',  ( 0.3139855153997000436, 24.38894642224000009, 2.697844032124999902 ) ) ;
#15362 = CARTESIAN_POINT ( 'NONE',  ( 14.20013902425123575, -8.115563385662030171, -6.363435485192806773 ) ) ;
#15363 = ORIENTED_EDGE ( 'NONE', *, *, #19725, .F. ) ;
#15364 = FACE_OUTER_BOUND ( 'NONE', #1029, .T. ) ;
#15365 = CARTESIAN_POINT ( 'NONE',  ( 5.625000000000000000, 21.50000000000000000, 1.676175670483999962E-09 ) ) ;
#15366 = EDGE_CURVE ( 'NONE', #12621, #19254, #13002, .T. ) ;
#15367 = FACE_OUTER_BOUND ( 'NONE', #4932, .T. ) ;
#15368 = CARTESIAN_POINT ( 'NONE',  ( 11.29022434642157791, 2.380282113839690794, 12.49997383652757144 ) ) ;
#15369 = DIRECTION ( 'NONE',  ( -1.000000000000000000, 0.000000000000000000, 0.000000000000000000 ) ) ;
#15370 = FACE_OUTER_BOUND ( 'NONE', #20400, .T. ) ;
#15371 = CARTESIAN_POINT ( 'NONE',  ( -21.32287077250664709, 5.665269408240008353, -7.371613913343743718 ) ) ;
#15372 = CARTESIAN_POINT ( 'NONE',  ( -2.500000000000000000, 26.50000000000000355, 0.000000000000000000 ) ) ;
#15373 = ORIENTED_EDGE ( 'NONE', *, *, #8228, .T. ) ;
#15374 = DIRECTION ( 'NONE',  ( 0.000000000000000000, 1.000000000000000000, 0.000000000000000000 ) ) ;
#15375 = AXIS2_PLACEMENT_3D ( 'NONE', #9034, #21989, #12440 ) ;
#15376 = ORIENTED_EDGE ( 'NONE', *, *, #10608, .F. ) ;
#15377 = B_SPLINE_CURVE_WITH_KNOTS ( 'NONE', 3,
 ( #7455, #18260, #20083, #5768, #16424, #23813, #14954, #1901, #12806, #13154, #5423, #20547, #10985, #12912, #18489, #20194, #16665, #1780, #18612, #20428, #3837, #16775, #71, #1662, #5302, #184, #12692, #7344, #3603, #2131, #9169, #14838, #9520, #5531 ),
 .UNSPECIFIED., .F., .F.,
 ( 4, 2, 2, 2, 2, 2, 2, 2, 2, 2, 2, 2, 2, 2, 2, 2, 4 ),
 ( 0.000000000000000000, 0.06249999999999997224, 0.1249999999999999445, 0.1874999999999999167, 0.2499999999999998890, 0.3124999999999998890, 0.3749999999999998335, 0.4374999999999998335, 0.4999999999999998890, 0.5624999999999998890, 0.6249999999999997780, 0.6874999999999997780, 0.7499999999999998890, 0.8125000000000000000, 0.8750000000000000000, 0.9375000000000000000, 1.000000000000000000 ),
 .UNSPECIFIED. ) ;
#15378 = PRODUCT_DEFINITION_SHAPE ( 'NONE', 'NONE',  #23971 ) ;
#15379 = CARTESIAN_POINT ( 'NONE',  ( -2.685167613138000231, 25.68485474111000144, 0.5308767225436000770 ) ) ;
#15381 = DIRECTION ( 'NONE',  ( 0.000000000000000000, 0.3197346865517833869, -0.9475071135435515490 ) ) ;
#15380 = CARTESIAN_POINT ( 'NONE',  ( -2.711598292089676399, 11.79220046658777044, 3.994969842139935334 ) ) ;
#15382 = CARTESIAN_POINT ( 'NONE',  ( 0.4554420578654839735, 24.53874986669016778, 2.337013420279270726 ) ) ;
#15383 = CARTESIAN_POINT ( 'NONE',  ( 14.41117308877000092, -6.232064677282999732, -9.080323572665999876 ) ) ;
#15384 = CARTESIAN_POINT ( 'NONE',  ( -6.382276157104002756, 15.08198816355999128, -3.360859746888000377 ) ) ;
#15385 = DIRECTION ( 'NONE',  ( 0.000000000000000000, 0.000000000000000000, 1.000000000000000000 ) ) ;
#15386 = ORIENTED_EDGE ( 'NONE', *, *, #4462, .T. ) ;
#15387 = ORIENTED_EDGE ( 'NONE', *, *, #1963, .T. ) ;
#15388 = CARTESIAN_POINT ( 'NONE',  ( -14.00000000000000711, -1.908289287512767052, -9.413725350966782202 ) ) ;
#15389 = VECTOR ( 'NONE', #7690, 1000.000000000000227 ) ;
#15390 = CARTESIAN_POINT ( 'NONE',  ( 3.000000000000000000, 20.10000000000000142, 0.000000000000000000 ) ) ;
#15391 = CARTESIAN_POINT ( 'NONE',  ( -14.44097978627332601, -9.338505494777370686, -8.825220280763023339 ) ) ;
#15392 = VERTEX_POINT ( 'NONE', #11078 ) ;
#15393 = CARTESIAN_POINT ( 'NONE',  ( 1.699999998837999904, 12.90000000000000036, -1.053565373074999867 ) ) ;
#15394 = DIRECTION ( 'NONE',  ( 0.000000000000000000, 0.000000000000000000, -1.000000000000000000 ) ) ;
#15395 = CARTESIAN_POINT ( 'NONE',  ( 15.25733488771729363, 3.913752835213978098, 9.572631007212564214 ) ) ;
#15396 = CIRCLE ( 'NONE', #12332, 0.09999999999999939493 ) ;
#15397 = CARTESIAN_POINT ( 'NONE',  ( -18.70603407209999958, 11.04749776926000138, -1.268528793046000080 ) ) ;
#15398 = EDGE_CURVE ( 'NONE', #12379, #953, #17274, .T. ) ;
#15399 = CARTESIAN_POINT ( 'NONE',  ( 2.220168113581999947, 28.86544355015000107, -0.7890638476296999437 ) ) ;
#15400 = CARTESIAN_POINT ( 'NONE',  ( -21.15342916351980662, -9.631976845097828033, -4.232284332473250643 ) ) ;
#15401 = CARTESIAN_POINT ( 'NONE',  ( -13.36117685223999985, -10.17969989951000009, -0.7718705306884999784 ) ) ;
#15402 = CONICAL_SURFACE ( 'NONE', #18136, 2.249999993279999888, 0.7853981633972997312 ) ;
#15403 = CARTESIAN_POINT ( 'NONE',  ( -0.5680056327079126000, 29.56997042186494795, 2.083912535968097224 ) ) ;
#15404 = EDGE_LOOP ( 'NONE', ( #22389, #23318, #15221, #10779, #6858 ) ) ;
#15405 = CARTESIAN_POINT ( 'NONE',  ( 0.9838067277388000686, 24.96693921933999860, -2.132932039142000136 ) ) ;
#15406 = CARTESIAN_POINT ( 'NONE',  ( -12.00000000000000000, -7.000000000000000000, 0.000000000000000000 ) ) ;
#15407 = AXIS2_PLACEMENT_3D ( 'NONE', #22722, #19220, #22606 ) ;
#15408 = ORIENTED_EDGE ( 'NONE', *, *, #13633, .T. ) ;
#15409 = CARTESIAN_POINT ( 'NONE',  ( 6.082094348699005337, 14.07676700545000159, -0.0001361385119140001254 ) ) ;
#15410 = ADVANCED_FACE ( 'NONE', ( #16158 ), #19209, .F. ) ;
#15411 = CARTESIAN_POINT ( 'NONE',  ( -2.125654151014383153, 30.86397478161066843, 0.2102433260543445648 ) ) ;
#15412 = AXIS2_PLACEMENT_3D ( 'NONE', #11054, #9119, #16492 ) ;
#15413 = CARTESIAN_POINT ( 'NONE',  ( -20.40997087121332498, -9.195041791531188835, -1.203755103560655515 ) ) ;
#15414 = CARTESIAN_POINT ( 'NONE',  ( 11.96718892131000089, -1.481964887125999830, -9.481920936164000224 ) ) ;
#15415 = ORIENTED_EDGE ( 'NONE', *, *, #1985, .F. ) ;
#15416 = CARTESIAN_POINT ( 'NONE',  ( -6.046766738174004452, 15.84711126475002274, -1.061654000538000409 ) ) ;
#15417 = CARTESIAN_POINT ( 'NONE',  ( -1.181632374603359237, 24.55137445130588958, -3.936586548166618460 ) ) ;
#15418 = LINE ( 'NONE', #2351, #3363 ) ;
#15419 = CIRCLE ( 'NONE', #5019, 4.000000000000000000 ) ;
#15420 = ORIENTED_EDGE ( 'NONE', *, *, #21994, .T. ) ;
#15421 = FACE_OUTER_BOUND ( 'NONE', #22645, .T. ) ;
#15422 = LINE ( 'NONE', #10108, #831 ) ;
#15423 = DIRECTION ( 'NONE',  ( 0.000000000000000000, 0.000000000000000000, -1.000000000000000000 ) ) ;
#15424 = DIRECTION ( 'NONE',  ( 0.000000000000000000, 0.8075558440518585401, 0.5897911144953695839 ) ) ;
#15426 = CARTESIAN_POINT ( 'NONE',  ( 18.32130157512671431, 7.445732629929010749, -7.287811148872539668 ) ) ;
#15425 = AXIS2_PLACEMENT_3D ( 'NONE', #18953, #11577, #17136 ) ;
#15427 = CARTESIAN_POINT ( 'NONE',  ( 12.00000000000000000, -6.392339033789701475, -7.402648988114485462 ) ) ;
#15428 = EDGE_CURVE ( 'NONE', #9475, #2076, #20170, .T. ) ;
#15429 = CARTESIAN_POINT ( 'NONE',  ( 18.81024770046333217, -7.320231837943222075, -5.625464605131847762 ) ) ;
#15430 = CARTESIAN_POINT ( 'NONE',  ( -3.336044988794002020, 13.59222169570000815, -5.136926126623002631 ) ) ;
#15431 = DIRECTION ( 'NONE',  ( -1.000000000000000000, 0.000000000000000000, 0.000000000000000000 ) ) ;
#15432 = AXIS2_PLACEMENT_3D ( 'NONE', #21390, #10248, #10007 ) ;
#15433 = CARTESIAN_POINT ( 'NONE',  ( -1.999167105995453442, 28.95086340285666182, -1.536366799937283645 ) ) ;
#15434 = CARTESIAN_POINT ( 'NONE',  ( 2.500000000000000000, 27.83419673618999823, 0.000000000000000000 ) ) ;
#15435 = CARTESIAN_POINT ( 'NONE',  ( -0.1289249096770258562, 30.39619859440238159, 2.156031166653296971 ) ) ;
#15436 = ORIENTED_EDGE ( 'NONE', *, *, #4475, .F. ) ;
#15437 = CARTESIAN_POINT ( 'NONE',  ( 24.39041767111999803, -3.750290925976000000, 10.88138972583000097 ) ) ;
#15438 = CARTESIAN_POINT ( 'NONE',  ( -3.913786546566217606, 13.31583390095716091, -5.570166324937983582 ) ) ;
#15439 = PLANE ( 'NONE',  #7649 ) ;
#15440 = VECTOR ( 'NONE', #370, 1000.000000000000000 ) ;
#15441 = CARTESIAN_POINT ( 'NONE',  ( -20.93881454081395432, -9.385637307247952421, -4.751717301100214286 ) ) ;
#15442 = CARTESIAN_POINT ( 'NONE',  ( -1.954613887214999846, 25.91864211381999894, -1.197800277839999872 ) ) ;
#15443 = ADVANCED_FACE ( 'NONE', ( #1755 ), #20284, .T. ) ;
#15444 = VECTOR ( 'NONE', #6300, 1000.000000000000000 ) ;
#15445 = CARTESIAN_POINT ( 'NONE',  ( 12.52688711657000020, -7.716878364870000340, 11.63397459621999985 ) ) ;
#15446 = ORIENTED_EDGE ( 'NONE', *, *, #3187, .F. ) ;
#15447 = CARTESIAN_POINT ( 'NONE',  ( -17.20986988650785676, -7.119360151369234835, -7.611991465795363787 ) ) ;
#15448 = CARTESIAN_POINT ( 'NONE',  ( -11.99999999434999864, 6.999999994347000154, 4.083276180409999442E-09 ) ) ;
#15449 = CARTESIAN_POINT ( 'NONE',  ( 1.473293862388198594, 28.13663838358920088, -1.634089070379382891 ) ) ;
#15450 = CARTESIAN_POINT ( 'NONE',  ( -10.25814758309999952, 1.350272875175999940E-14, 0.000000000000000000 ) ) ;
#15451 = VERTEX_POINT ( 'NONE', #12883 ) ;
#15452 = CARTESIAN_POINT ( 'NONE',  ( -7.834000000000000519, 1.320585629393000037E-14, 0.000000000000000000 ) ) ;
#15453 = CARTESIAN_POINT ( 'NONE',  ( 18.27225174930999785, 9.757448129154999705, -4.584997352848999341 ) ) ;
#15454 = CARTESIAN_POINT ( 'NONE',  ( -14.11822151763998967, 4.169118407994018227, -8.067165099063066336 ) ) ;
#15455 = EDGE_CURVE ( 'NONE', #20876, #15263, #2973, .T. ) ;
#15456 = CARTESIAN_POINT ( 'NONE',  ( -14.54749130609000041, 5.065910023622000047, 10.11535946923000040 ) ) ;
#15457 = DIRECTION ( 'NONE',  ( -0.000000000000000000, 1.000000000000000000, 0.000000000000000000 ) ) ;
#15458 = EDGE_CURVE ( 'NONE', #7505, #20171, #23069, .T. ) ;
#15459 = CARTESIAN_POINT ( 'NONE',  ( 16.68171080085999947, 11.38129333810999988, 0.2944024164967999901 ) ) ;
#15460 = CARTESIAN_POINT ( 'NONE',  ( -0.8766499437396024774, 28.75150226347701476, 1.987951473063243935 ) ) ;
#15461 = DIRECTION ( 'NONE',  ( 1.000000000000000000, 0.000000000000000000, 0.000000000000000000 ) ) ;
#15462 = CARTESIAN_POINT ( 'NONE',  ( 20.31311216239999951, -2.731102875616999714, -9.830470219947999411 ) ) ;
#15463 = CARTESIAN_POINT ( 'NONE',  ( -2.500000000000000000, 26.63419673618999894, 0.000000000000000000 ) ) ;
#15464 = EDGE_LOOP ( 'NONE', ( #19124, #14599, #14400, #4101 ) ) ;
#15465 = CARTESIAN_POINT ( 'NONE',  ( 11.89062890675000084, 5.534444999978999746, -7.067249179718999130 ) ) ;
#15466 = CARTESIAN_POINT ( 'NONE',  ( 1.099251314038999894, 29.01456776952000283, 2.157402177123000087 ) ) ;
#15467 = CIRCLE ( 'NONE', #5060, 0.5500000000000001554 ) ;
#15468 = CARTESIAN_POINT ( 'NONE',  ( -4.671193161643005354, 12.51559483494999192, 0.7204251727433007568 ) ) ;
#15469 = CARTESIAN_POINT ( 'NONE',  ( 1.439764776165384008, 28.89522456450965038, 1.649428253125927668 ) ) ;
#15470 = CARTESIAN_POINT ( 'NONE',  ( -20.45236390540999949, 6.914456025393000083, -8.636057584528000319 ) ) ;
#15471 = VERTEX_POINT ( 'NONE', #1637 ) ;
#15472 = EDGE_CURVE ( 'NONE', #9272, #12394, #20379, .T. ) ;
#15473 = EDGE_CURVE ( 'NONE', #22015, #9475, #16493, .T. ) ;
#15474 = DIRECTION ( 'NONE',  ( 0.000000000000000000, 1.000000000000000000, 0.000000000000000000 ) ) ;
#15475 = EDGE_LOOP ( 'NONE', ( #20752, #12139, #10897, #2023, #21786, #20131, #12803 ) ) ;
#15476 = CARTESIAN_POINT ( 'NONE',  ( 14.99328936713000004, -9.056039068417000237, 0.000000000000000000 ) ) ;
#15477 = LINE ( 'NONE', #15226, #3145 ) ;
#15478 = CARTESIAN_POINT ( 'NONE',  ( -3.476879115686000166, 13.24153924759999867, 5.444655603229995755 ) ) ;
#15479 = DIRECTION ( 'NONE',  ( 1.000000000000000000, 0.000000000000000000, 0.000000000000000000 ) ) ;
#15480 = LINE ( 'NONE', #21308, #8382 ) ;
#15481 = CARTESIAN_POINT ( 'NONE',  ( -19.08958467661999947, -10.87501988123999830, 0.7812661330421999395 ) ) ;
#15482 = CARTESIAN_POINT ( 'NONE',  ( 12.70856375730999943, -1.114725866925000197, 9.038927914362998806 ) ) ;
#15483 = CARTESIAN_POINT ( 'NONE',  ( 2.500000000000001776, 27.58333333333333570, 0.3272492347489265874 ) ) ;
#15484 = VERTEX_POINT ( 'NONE', #4183 ) ;
#15485 = FACE_OUTER_BOUND ( 'NONE', #11435, .T. ) ;
#15486 = CARTESIAN_POINT ( 'NONE',  ( 0.01985994072882999936, 24.87862773921999704, -2.525494120218000127 ) ) ;
#15487 = CARTESIAN_POINT ( 'NONE',  ( 13.84634332888274244, -8.698285480931694735, 5.523431346751156212 ) ) ;
#15488 = CIRCLE ( 'NONE', #8945, 3.100000000000000089 ) ;
#15489 = VERTEX_POINT ( 'NONE', #21014 ) ;
#15490 = CARTESIAN_POINT ( 'NONE',  ( -3.088892724819999103, 14.26228888334000366, -5.340567897133000841 ) ) ;
#15491 = DIRECTION ( 'NONE',  ( -3.122502256758250246E-14, 1.000000000000000000, 0.000000000000000000 ) ) ;
#15492 = CARTESIAN_POINT ( 'NONE',  ( 1.932766431522000117, 28.47362202384999819, 1.950198670200999906 ) ) ;
#15493 = CARTESIAN_POINT ( 'NONE',  ( 11.43887872963242103, -3.075720902669945023, 12.49994001780760478 ) ) ;
#15494 = CARTESIAN_POINT ( 'NONE',  ( 17.06835809520467251, -2.939044901913968388, 10.00778562106659031 ) ) ;
#15495 = DIRECTION ( 'NONE',  ( 1.000000000000000000, 0.000000000000000000, 0.000000000000000000 ) ) ;
#15496 = CARTESIAN_POINT ( 'NONE',  ( -21.05832910583999862, 9.211679941677999750, 0.000000000000000000 ) ) ;
#15497 = DIRECTION ( 'NONE',  ( -1.000000000000000000, 0.000000000000000000, 0.000000000000000000 ) ) ;
#15498 = ORIENTED_EDGE ( 'NONE', *, *, #4777, .F. ) ;
#15499 = CARTESIAN_POINT ( 'NONE',  ( 11.18574820343724951, -9.950120879830603116, 7.765924039743827834 ) ) ;
#15500 = VERTEX_POINT ( 'NONE', #13263 ) ;
#15501 = DIRECTION ( 'NONE',  ( 0.000000000000000000, 0.000000000000000000, -1.000000000000000000 ) ) ;
#15503 = CARTESIAN_POINT ( 'NONE',  ( 2.031887307395044751, 24.15498103193775492, 0.8252474979483435114 ) ) ;
#15502 = CARTESIAN_POINT ( 'NONE',  ( 0.4218749374566191923, 11.48962318055099452, 4.794906470640148299 ) ) ;
#15504 = DIRECTION ( 'NONE',  ( 0.000000000000000000, 0.000000000000000000, -1.000000000000000000 ) ) ;
#15505 = CARTESIAN_POINT ( 'NONE',  ( -24.50000000000000000, 1.524685264937999788E-14, 0.000000000000000000 ) ) ;
#15506 = CARTESIAN_POINT ( 'NONE',  ( -6.445315760836000329, 15.10728987923999966, -3.240892097991999066 ) ) ;
#15507 = CARTESIAN_POINT ( 'NONE',  ( -6.838539683285000059, 15.31903379280000088, 1.878299112549000061 ) ) ;
#15508 = VERTEX_POINT ( 'NONE', #22699 ) ;
#15509 = VERTEX_POINT ( 'NONE', #6109 ) ;
#15510 = CARTESIAN_POINT ( 'NONE',  ( -13.99999999999999645, 1.096942893147169196, -9.373824115781612676 ) ) ;
#15511 = DIRECTION ( 'NONE',  ( 0.000000000000000000, 1.000000000000000000, 0.000000000000000000 ) ) ;
#15512 = CARTESIAN_POINT ( 'NONE',  ( 0.000000000000000000, -13.00000000000000000, 0.000000000000000000 ) ) ;
#15513 = ORIENTED_EDGE ( 'NONE', *, *, #22509, .T. ) ;
#15514 = CARTESIAN_POINT ( 'NONE',  ( -19.94541230731999804, -0.1261951200563999897, -9.624618949942000512 ) ) ;
#15515 = DIRECTION ( 'NONE',  ( 0.000000000000000000, -1.000000000000000000, 0.000000000000000000 ) ) ;
#15516 = CARTESIAN_POINT ( 'NONE',  ( 6.161504479767497600, 14.06289331633568374, 0.4242934236927147218 ) ) ;
#15517 = CARTESIAN_POINT ( 'NONE',  ( 15.68994637415852367, -9.253307702421135872, 4.643068743934705367 ) ) ;
#15518 = CARTESIAN_POINT ( 'NONE',  ( -14.04282959941999920, -10.81806137319999905, 1.946765347141999891 ) ) ;
#15519 = DIRECTION ( 'NONE',  ( 0.000000000000000000, 0.000000000000000000, 1.000000000000000000 ) ) ;
#15520 = CARTESIAN_POINT ( 'NONE',  ( -20.81887252879722894, 0.02655197213427299210, -10.51206043786136846 ) ) ;
#15521 = CARTESIAN_POINT ( 'NONE',  ( -16.69277858220999988, 10.68419017778999880, -3.897213304429000491 ) ) ;
#15522 = AXIS2_PLACEMENT_3D ( 'NONE', #23293, #23413, #4908 ) ;
#15523 = B_SPLINE_CURVE_WITH_KNOTS ( 'NONE', 3,
 ( #10324, #19652, #6437, #985 ),
 .UNSPECIFIED., .F., .F.,
 ( 4, 4 ),
 ( 0.000000000000000000, 1.000000000000000000 ),
 .UNSPECIFIED. ) ;
#15524 = CARTESIAN_POINT ( 'NONE',  ( -0.5273013900716050362, 29.57247171166937605, 2.094731424541075526 ) ) ;
#15525 = ORIENTED_EDGE ( 'NONE', *, *, #14735, .T. ) ;
#15526 = CARTESIAN_POINT ( 'NONE',  ( -1.677508373566000133, 23.67725715092000272, 1.401457983775999949 ) ) ;
#15527 = CARTESIAN_POINT ( 'NONE',  ( -15.59164245049265496, -7.009879148460222531, -7.667866936169112080 ) ) ;
#15528 = ORIENTED_EDGE ( 'NONE', *, *, #9269, .F. ) ;
#15529 = CARTESIAN_POINT ( 'NONE',  ( -2.191702116096594821, 24.63208194274876917, -0.6023946256753694994 ) ) ;
#15530 = CARTESIAN_POINT ( 'NONE',  ( 5.805692032784003587, 13.82232033692000428, -2.386350607328999729 ) ) ;
#15531 = CARTESIAN_POINT ( 'NONE',  ( -2.123582770898495120, 30.87008440628623873, 0.1642131033563037079 ) ) ;
#15532 = DIRECTION ( 'NONE',  ( -1.000000000000000000, 0.000000000000000000, 0.000000000000000000 ) ) ;
#15533 = ADVANCED_FACE ( 'NONE', ( #13616 ), #22344, .T. ) ;
#15534 = CARTESIAN_POINT ( 'NONE',  ( 18.02643908530999894, 9.290813243320000581, -4.365746228316999655 ) ) ;
#15535 = ORIENTED_EDGE ( 'NONE', *, *, #9210, .T. ) ;
#15536 = FACE_OUTER_BOUND ( 'NONE', #6687, .T. ) ;
#15537 = CARTESIAN_POINT ( 'NONE',  ( 24.24531177150999994, 0.000000000000000000, 0.000000000000000000 ) ) ;
#15538 = CARTESIAN_POINT ( 'NONE',  ( 24.50000000000000000, -11.33659675998026728, 5.364438426793228132 ) ) ;
#15539 = VERTEX_POINT ( 'NONE', #13502 ) ;
#15540 = CARTESIAN_POINT ( 'NONE',  ( -4.549999999999999822, 24.49999999999999645, 0.000000000000000000 ) ) ;
#15541 = CARTESIAN_POINT ( 'NONE',  ( 11.90008533512019717, 8.504566836169448862, 10.26973740115608535 ) ) ;
#15542 = DIRECTION ( 'NONE',  ( 0.000000000000000000, 1.000000000000000000, 0.000000000000000000 ) ) ;
#15543 = AXIS2_PLACEMENT_3D ( 'NONE', #31, #15149, #20388 ) ;
#15544 = CARTESIAN_POINT ( 'NONE',  ( 4.000000000000000888, 26.37418302490048561, 1.506880184559474811 ) ) ;
#15545 = CARTESIAN_POINT ( 'NONE',  ( 18.32319020317524760, 7.491395659936667784, -7.241007325533137085 ) ) ;
#15546 = CARTESIAN_POINT ( 'NONE',  ( 12.00000000000000711, -7.523096633965199231, -6.369279415753941187 ) ) ;
#15547 = ADVANCED_FACE ( 'NONE', ( #2607, #2126 ), #3953, .F. ) ;
#15548 = DIRECTION ( 'NONE',  ( 0.000000000000000000, 1.000000000000000000, 0.000000000000000000 ) ) ;
#15549 = CARTESIAN_POINT ( 'NONE',  ( 20.08785956010000007, 11.04335702312000045, 1.829420851330999964 ) ) ;
#15550 = CARTESIAN_POINT ( 'NONE',  ( -1.350914310362234527, 26.47444252552741872, 3.838851412777818606 ) ) ;
#15551 = CARTESIAN_POINT ( 'NONE',  ( -3.932855452960560605, 13.92334204325285363, -4.847046887875868570 ) ) ;
#15552 = DIRECTION ( 'NONE',  ( -1.000000000000000000, 0.000000000000000000, 0.000000000000000000 ) ) ;
#15553 = CARTESIAN_POINT ( 'NONE',  ( -0.9850774032204228092, 30.06393871203397339, -1.927287055198054322 ) ) ;
#15554 = ORIENTED_EDGE ( 'NONE', *, *, #5142, .T. ) ;
#15555 = CARTESIAN_POINT ( 'NONE',  ( 21.96628300751999774, 0.8142437358098000288, 10.33950846541999979 ) ) ;
#15556 = CARTESIAN_POINT ( 'NONE',  ( -2.908727297478219231, 13.08990433425206312, -6.081832042887836742 ) ) ;
#15557 = CARTESIAN_POINT ( 'NONE',  ( 1.999167105995457216, 27.75086340285666608, 1.536366799937278760 ) ) ;
#15558 = CARTESIAN_POINT ( 'NONE',  ( -19.70710128986670284, -0.2415848317640648391, 10.48256611230249291 ) ) ;
#15559 = CARTESIAN_POINT ( 'NONE',  ( -12.50000000000000000, 1.377727649040999975E-14, 0.000000000000000000 ) ) ;
#15560 = AXIS2_PLACEMENT_3D ( 'NONE', #2565, #15515, #19285 ) ;
#15561 = CARTESIAN_POINT ( 'NONE',  ( -6.281924650935041932, 26.47351824524191954, 1.064721106944196416 ) ) ;
#15562 = ORIENTED_EDGE ( 'NONE', *, *, #17390, .F. ) ;
#15563 = ADVANCED_FACE ( 'NONE', ( #17260 ), #20655, .F. ) ;
#15564 = CARTESIAN_POINT ( 'NONE',  ( -16.90284627698810027, 3.185908784686084960, -9.919433582464312948 ) ) ;
#15565 = CARTESIAN_POINT ( 'NONE',  ( 4.750000000000000000, 22.19999999999999574, 0.000000000000000000 ) ) ;
#15566 = CARTESIAN_POINT ( 'NONE',  ( -1.908614330669104797, 27.69283736032755172, 1.033640524002992667 ) ) ;
#15567 = DIRECTION ( 'NONE',  ( 1.000000000000000000, 0.000000000000000000, 0.000000000000000000 ) ) ;
#15568 = VERTEX_POINT ( 'NONE', #4306 ) ;
#15569 = CARTESIAN_POINT ( 'NONE',  ( 16.88287270046333433, -8.867611548585280445, -2.382974050612994610 ) ) ;
#15570 = CARTESIAN_POINT ( 'NONE',  ( 15.74943924931000083, -10.38900229657999930, -2.621660623529000311 ) ) ;
#15571 = CARTESIAN_POINT ( 'NONE',  ( -22.13189778338000124, 11.16819092355999921, -0.3469374994123999856 ) ) ;
#15572 = EDGE_CURVE ( 'NONE', #19752, #14691, #658, .T. ) ;
#15573 = CARTESIAN_POINT ( 'NONE',  ( -14.88272252886000047, -2.429795583095000211, 9.959192131528999070 ) ) ;
#15574 = CARTESIAN_POINT ( 'NONE',  ( 0.000000000000000000, 24.50000000000000000, 0.000000000000000000 ) ) ;
#15575 = CARTESIAN_POINT ( 'NONE',  ( 13.77119494526000132, 8.252143983288998896, 6.036643158187999347 ) ) ;
#15576 = CARTESIAN_POINT ( 'NONE',  ( -14.25623308043999948, -13.93375672974000068, -0.4324171310913000332 ) ) ;
#15577 = CARTESIAN_POINT ( 'NONE',  ( 1.259047450927257339, 26.90086340285667177, 2.184465970885639763 ) ) ;
#15578 = CARTESIAN_POINT ( 'NONE',  ( 21.29261314321999876, 7.944215266713999135, 5.566623593713999618 ) ) ;
#15579 = PRODUCT ( 'Rotary Valve Ball', 'Rotary Valve Ball', '', ( #17523 ) ) ;
#15580 = DIRECTION ( 'NONE',  ( 0.000000000000000000, 1.000000000000000000, 0.000000000000000000 ) ) ;
#15581 = ORIENTED_EDGE ( 'NONE', *, *, #23747, .T. ) ;
#15582 = CARTESIAN_POINT ( 'NONE',  ( -2.717159071278044902, 14.05084818344029962, 5.491236865063197747 ) ) ;
#15583 = CARTESIAN_POINT ( 'NONE',  ( 1.304555153736000062, 26.08956776952000212, -2.329463490920999913 ) ) ;
#15584 = CARTESIAN_POINT ( 'NONE',  ( 0.8118633353224987692, 11.52213133294999459, 4.737706653456997152 ) ) ;
#15585 = EDGE_CURVE ( 'NONE', #18186, #9739, #11696, .T. ) ;
#15586 = CARTESIAN_POINT ( 'NONE',  ( 2.013606499909832426, 28.95625055469338349, 0.7894195048039055473 ) ) ;
#15587 = CARTESIAN_POINT ( 'NONE',  ( 0.1442055869094999998, 27.60687716035999983, -2.445277951317000209 ) ) ;
#15588 = FACE_OUTER_BOUND ( 'NONE', #10356, .T. ) ;
#15589 = VERTEX_POINT ( 'NONE', #8062 ) ;
#15590 = CARTESIAN_POINT ( 'NONE',  ( 15.29562270046331740, -4.564817758524311486, -7.919774334405468075 ) ) ;
#15591 = EDGE_CURVE ( 'NONE', #15625, #20267, #9514, .T. ) ;
#15592 = DIRECTION ( 'NONE',  ( 0.8660254037844288266, 0.5000000000000169864, 0.000000000000000000 ) ) ;
#15593 = CARTESIAN_POINT ( 'NONE',  ( -4.353590520638998207, 13.53542079822999256, 4.749304138607999271 ) ) ;
#15594 = EDGE_CURVE ( 'NONE', #20706, #10102, #18637, .T. ) ;
#15595 = CARTESIAN_POINT ( 'NONE',  ( 0.2041544774629323045, 6.780677947102329739, 1.738509534568517090 ) ) ;
#15596 = CARTESIAN_POINT ( 'NONE',  ( 0.000000000000000000, 26.20000000000000284, 4.618802153517000519 ) ) ;
#15597 = AXIS2_PLACEMENT_3D ( 'NONE', #19311, #8541, #8652 ) ;
#15598 = CARTESIAN_POINT ( 'NONE',  ( -6.046837210729000489, 16.30334039894000142, -1.000000000000000000 ) ) ;
#15599 = CARTESIAN_POINT ( 'NONE',  ( 14.24418875730999900, 6.821019272440999259, 6.095525253705999624 ) ) ;
#15600 = CARTESIAN_POINT ( 'NONE',  ( 1.999167105995457661, 27.51666666666667282, 1.536366799937278760 ) ) ;
#15601 = ORIENTED_EDGE ( 'NONE', *, *, #6572, .T. ) ;
#15602 = EDGE_CURVE ( 'NONE', #15754, #9702, #18956, .T. ) ;
#15603 = CARTESIAN_POINT ( 'NONE',  ( 19.94084516911093630, 7.608551632648391738, -7.249783728510496239 ) ) ;
#15604 = CARTESIAN_POINT ( 'NONE',  ( -2.185797623742999907, 30.54140998917999994, 1.625295296457000216 ) ) ;
#15605 = CARTESIAN_POINT ( 'NONE',  ( 2.069451752920999699, 23.68449416383000283, 1.759067238232999930 ) ) ;
#15606 = CARTESIAN_POINT ( 'NONE',  ( 1.406122888814909988, 13.78777984639410548, -5.962141027037247021 ) ) ;
#15607 = CARTESIAN_POINT ( 'NONE',  ( 4.921628875838995221, 13.75323042666000362, -4.185280411400999157 ) ) ;
#15608 = DIRECTION ( 'NONE',  ( 0.000000000000000000, 0.000000000000000000, -1.000000000000000000 ) ) ;
#15609 = CARTESIAN_POINT ( 'NONE',  ( 14.65997133257774543, -8.964114299601121161, 1.438260584116868079 ) ) ;
#15610 = CARTESIAN_POINT ( 'NONE',  ( 16.87321770986947556, 3.972702165366156279, 9.639322115070482866 ) ) ;
#15611 = CARTESIAN_POINT ( 'NONE',  ( 23.75352077758000036, 36.75000000000000000, -6.000000000000000000 ) ) ;
#15612 = CARTESIAN_POINT ( 'NONE',  ( 0.000000000000000000, 17.00000000000000000, 0.000000000000000000 ) ) ;
#15613 = AXIS2_PLACEMENT_3D ( 'NONE', #9710, #9472, #16617 ) ;
#15614 = CARTESIAN_POINT ( 'NONE',  ( 0.000000000000000000, 18.50000000000000000, 0.000000000000000000 ) ) ;
#15615 = ORIENTED_EDGE ( 'NONE', *, *, #21850, .F. ) ;
#15616 = DIRECTION ( 'NONE',  ( 0.000000000000000000, 0.000000000000000000, -1.000000000000000000 ) ) ;
#15617 = CARTESIAN_POINT ( 'NONE',  ( 11.66614181941011985, -8.864734480512577619, 9.645689288213576518 ) ) ;
#15618 = ORIENTED_EDGE ( 'NONE', *, *, #6996, .T. ) ;
#15619 = DIRECTION ( 'NONE',  ( -0.9970458808888235103, 0.000000000000000000, -0.07680827691486176445 ) ) ;
#15620 = CARTESIAN_POINT ( 'NONE',  ( -1.660235382367824641, 24.69477898227424006, 1.432877587170922284 ) ) ;
#15621 = CARTESIAN_POINT ( 'NONE',  ( -2.964817197442055186, 13.10038421424571276, 6.059153498010348748 ) ) ;
#15622 = CARTESIAN_POINT ( 'NONE',  ( -4.900699999999999612, 1.284663064832999817E-14, 0.000000000000000000 ) ) ;
#15623 = CARTESIAN_POINT ( 'NONE',  ( 66.60588651278291650, 37.01856778792605240, -1.000000000000000000 ) ) ;
#15624 = ORIENTED_EDGE ( 'NONE', *, *, #3593, .T. ) ;
#15625 = VERTEX_POINT ( 'NONE', #296 ) ;
#15626 = CARTESIAN_POINT ( 'NONE',  ( -14.00000000000000711, -7.717499669629955150, -6.307697564917725153 ) ) ;
#15627 = CONICAL_SURFACE ( 'NONE', #11398, 9.152445778720998959, 0.02565634000431304615 ) ;
#15628 = CARTESIAN_POINT ( 'NONE',  ( 13.21250000000000036, 0.000000000000000000, 0.000000000000000000 ) ) ;
#15629 = EDGE_LOOP ( 'NONE', ( #11491, #14991, #17757, #23439 ) ) ;
#15630 = EDGE_CURVE ( 'NONE', #23948, #2047, #23466, .T. ) ;
#15631 = CARTESIAN_POINT ( 'NONE',  ( -20.97361272096999940, 4.049795877874999839, 8.762865524082998903 ) ) ;
#15632 = LINE ( 'NONE', #15393, #20235 ) ;
#15633 = CARTESIAN_POINT ( 'NONE',  ( 6.168359549731804670, 14.02575663701962760, 0.5147778748295055440 ) ) ;
#15634 = CARTESIAN_POINT ( 'NONE',  ( 15.14759469764988786, 7.222759206179429015, 7.395737098632818807 ) ) ;
#15635 = CARTESIAN_POINT ( 'NONE',  ( -13.86216628438999976, -9.279585093157001197, -4.454637058083000589 ) ) ;
#15636 = CARTESIAN_POINT ( 'NONE',  ( 11.49999999537000051, 6.999999995366000149, 1.987950376480999949E-09 ) ) ;
#15637 = CARTESIAN_POINT ( 'NONE',  ( -21.61666142697704629, -3.977296262259868431, 9.886869024158263741 ) ) ;
#15638 = CARTESIAN_POINT ( 'NONE',  ( -15.67712684235999987, -11.34047394370000106, -0.3014134449561000073 ) ) ;
#15639 = CARTESIAN_POINT ( 'NONE',  ( -0.9423453617915489300, 29.54624551692468160, 1.944123615020682427 ) ) ;
#15640 = EDGE_LOOP ( 'NONE', ( #2952, #3268, #18718 ) ) ;
#15641 = CARTESIAN_POINT ( 'NONE',  ( -2.323275342901000240, 23.64078167485000037, 0.3458804795797000287 ) ) ;
#15642 = AXIS2_PLACEMENT_3D ( 'NONE', #16220, #12597, #19983 ) ;
#15643 = CARTESIAN_POINT ( 'NONE',  ( -16.19936510130885665, -3.025408273704439210, 9.955618328560920105 ) ) ;
#15644 = EDGE_LOOP ( 'NONE', ( #5969, #17686 ) ) ;
#15645 = LINE ( 'NONE', #2460, #23434 ) ;
#15646 = CARTESIAN_POINT ( 'NONE',  ( 6.131636900325998951, 14.49487543762001351, -0.1732800415016998163 ) ) ;
#15647 = CARTESIAN_POINT ( 'NONE',  ( 1.181632374602280988, 28.05137445130629104, 3.936586548167761990 ) ) ;
#15648 = DIRECTION ( 'NONE',  ( 1.000000000000000000, 0.000000000000000000, 0.000000000000000000 ) ) ;
#15649 = CARTESIAN_POINT ( 'NONE',  ( 14.92875142131000210, -6.069959421551999412, 7.533852356441999909 ) ) ;
#15650 = VERTEX_POINT ( 'NONE', #535 ) ;
#15651 = DIRECTION ( 'NONE',  ( 0.5000000000000169864, 0.000000000000000000, -0.8660254037844289376 ) ) ;
#15652 = B_SPLINE_CURVE_WITH_KNOTS ( 'NONE', 3,
 ( #16074, #6762, #23473, #14155, #10770, #12465, #3503, #10883, #18036, #23601, #18270, #14393, #1669, #1909, #9765, #22598, #9414, #2256 ),
 .UNSPECIFIED., .F., .F.,
 ( 4, 2, 2, 2, 2, 2, 2, 2, 4 ),
 ( 0.000000000000000000, 0.09877299861065136355, 0.1975459972213027271, 0.2963189958319540351, 0.3950919944426053987, 0.4938649930532567067, 0.5926379916639080703, 0.6914109902745593228, 0.7901839888852105753 ),
 .UNSPECIFIED. ) ;
#15653 = CARTESIAN_POINT ( 'NONE',  ( -2.184465970885646424, 27.13333333333333641, -1.259047450927245126 ) ) ;
#15654 = CARTESIAN_POINT ( 'NONE',  ( 3.649794085728313320, 24.70197603011190068, -2.511592555635393964 ) ) ;
#15655 = ORIENTED_EDGE ( 'NONE', *, *, #22715, .F. ) ;
#15656 = CARTESIAN_POINT ( 'NONE',  ( 4.000000000000000000, 26.24995697614769341, -2.103311180602513986 ) ) ;
#15657 = CARTESIAN_POINT ( 'NONE',  ( -3.657438266360000245, 84.95442836047000412, 3.657438266360000245 ) ) ;
#15658 = CARTESIAN_POINT ( 'NONE',  ( 24.02947265600820614, 7.126507592064388774, 7.874003420745752990 ) ) ;
#15659 = CIRCLE ( 'NONE', #976, 12.44999999999999929 ) ;
#15660 = CARTESIAN_POINT ( 'NONE',  ( -14.00000000000000000, -4.353401700033900035, 9.017588339353036275 ) ) ;
#15661 = CARTESIAN_POINT ( 'NONE',  ( 18.05830141818303147, -1.129169376018525961, -10.34964973624757789 ) ) ;
#15662 = DIRECTION ( 'NONE',  ( -1.000000000000000000, 0.000000000000000000, 0.000000000000000000 ) ) ;
#15663 = CARTESIAN_POINT ( 'NONE',  ( -14.38789256606429490, -8.761241120844353247, 9.824672794992769909 ) ) ;
#15664 = CARTESIAN_POINT ( 'NONE',  ( 22.84106400460000330, -10.84379783138999898, -3.067933783016000060 ) ) ;
#15665 = PLANE ( 'NONE',  #12548 ) ;
#15666 = CARTESIAN_POINT ( 'NONE',  ( -4.055068951189445770, 13.80018247765906025, -4.864706622278940351 ) ) ;
#15667 = CARTESIAN_POINT ( 'NONE',  ( -24.09039453749000259, 1.716648116605999814E-14, 0.000000000000000000 ) ) ;
#15668 = EDGE_CURVE ( 'NONE', #5299, #12159, #12262, .T. ) ;
#15669 = CARTESIAN_POINT ( 'NONE',  ( -1.903056763539824114, 30.14106874054843033, -1.021523276054197904 ) ) ;
#15670 = ORIENTED_EDGE ( 'NONE', *, *, #1552, .F. ) ;
#15671 = CARTESIAN_POINT ( 'NONE',  ( 20.42027553904000214, -7.757497012334000352, 6.819440105516999751 ) ) ;
#15672 = CARTESIAN_POINT ( 'NONE',  ( 24.21477607719004155, 7.477202524421422858, 7.546204228164135053 ) ) ;
#15673 = FACE_OUTER_BOUND ( 'NONE', #11599, .T. ) ;
#15674 = CARTESIAN_POINT ( 'NONE',  ( -19.49289028970277116, -7.253846718909587210, 7.562220539910094352 ) ) ;
#15675 = CONICAL_SURFACE ( 'NONE', #12987, 2.949999944334000368, 0.7853981633972997312 ) ;
#15676 = CARTESIAN_POINT ( 'NONE',  ( 4.903088169044051092, 14.37364044011246911, 3.818206020033084069 ) ) ;
#15677 = AXIS2_PLACEMENT_3D ( 'NONE', #18183, #20112, #23246 ) ;
#15678 = CARTESIAN_POINT ( 'NONE',  ( 4.620886678299001460, 12.32869312146999263, -1.717839858747998161 ) ) ;
#15679 = EDGE_LOOP ( 'NONE', ( #9474, #18937, #6211, #15525, #12156 ) ) ;
#15680 = CARTESIAN_POINT ( 'NONE',  ( -14.97697090817717935, 6.668094886919918807, -7.940777754376553865 ) ) ;
#15681 = CARTESIAN_POINT ( 'NONE',  ( -4.000000000000000000, 30.00000000000000000, 0.000000000000000000 ) ) ;
#15682 = CARTESIAN_POINT ( 'NONE',  ( -2.059085180431123874, 28.38319450762345753, -0.7814348820212547730 ) ) ;
#15683 = APPLICATION_PROTOCOL_DEFINITION ( 'draft international standard', 'automotive_design', 1998, #16691 ) ;
#15684 = DIRECTION ( 'NONE',  ( -1.000000000000000000, 0.000000000000000000, 0.000000000000000000 ) ) ;
#15685 = VERTEX_POINT ( 'NONE', #14109 ) ;
#15686 = CARTESIAN_POINT ( 'NONE',  ( 4.000000000000000000, 29.74995697614769341, -2.103311180602513542 ) ) ;
#15687 = CARTESIAN_POINT ( 'NONE',  ( 17.39475174931000012, -10.15246533026000186, 3.558175289345999914 ) ) ;
#15688 = CARTESIAN_POINT ( 'NONE',  ( -23.68577204849000140, -2.454364077398999644, 10.41095670075000079 ) ) ;
#15689 = CARTESIAN_POINT ( 'NONE',  ( -19.55472053216000106, -2.419448610677000122, -10.09555165608999872 ) ) ;
#15690 = CARTESIAN_POINT ( 'NONE',  ( -6.107093651952999913, 16.13547971460000596, 0.9717940814902004121 ) ) ;
#15691 = CARTESIAN_POINT ( 'NONE',  ( 14.24562451745999958, 2.264453579998999988, 9.429937331667000322 ) ) ;
#15692 = CARTESIAN_POINT ( 'NONE',  ( -3.999999999999999112, 26.49040384242090695, -0.4670641126940866528 ) ) ;
#15693 = AXIS2_PLACEMENT_3D ( 'NONE', #15099, #20455, #13060 ) ;
#15694 = CARTESIAN_POINT ( 'NONE',  ( -18.99854661335000117, 13.93375672974000068, 0.000000000000000000 ) ) ;
#15695 = ADVANCED_FACE ( 'NONE', ( #13988 ), #4914, .T. ) ;
#15696 = CARTESIAN_POINT ( 'NONE',  ( -23.74465998031000069, -7.716878364870000340, -11.63397459621999985 ) ) ;
#15697 = ORIENTED_EDGE ( 'NONE', *, *, #22063, .F. ) ;
#15698 = CARTESIAN_POINT ( 'NONE',  ( 0.000000000000000000, 22.09999988306815766, 0.000000000000000000 ) ) ;
#15699 = CARTESIAN_POINT ( 'NONE',  ( 1.402946323589000066, 26.19500240010000169, -2.505154520421000175 ) ) ;
#15700 = CARTESIAN_POINT ( 'NONE',  ( -4.720332369741998768, 12.53505228420999984, -0.1483533514531999165 ) ) ;
#15701 = CARTESIAN_POINT ( 'NONE',  ( 2.000000000000000000, 26.50000000000000355, 3.464101615137999968 ) ) ;
#15702 = CARTESIAN_POINT ( 'NONE',  ( -20.09773186494999919, 7.373291466226999269, 8.234872552958998781 ) ) ;
#15703 = DIRECTION ( 'NONE',  ( 0.000000000000000000, 1.000000000000000000, 0.000000000000000000 ) ) ;
#15704 = ORIENTED_EDGE ( 'NONE', *, *, #4777, .T. ) ;
#15705 = DIRECTION ( 'NONE',  ( 0.000000000000000000, 0.000000000000000000, -1.000000000000000000 ) ) ;
#15706 = LINE ( 'NONE', #13778, #20536 ) ;
#15707 = ADVANCED_FACE ( 'NONE', ( #21379 ), #21544, .F. ) ;
#15708 = CARTESIAN_POINT ( 'NONE',  ( -3.624149612674999243, 14.44537212523001202, 4.955916638659999762 ) ) ;
#15709 = AXIS2_PLACEMENT_3D ( 'NONE', #12222, #12463, #21304 ) ;
#15710 = CARTESIAN_POINT ( 'NONE',  ( 12.00000000000000000, 0.000000000000000000, 0.000000000000000000 ) ) ;
#15711 = LINE ( 'NONE', #704, #9963 ) ;
#15712 = CARTESIAN_POINT ( 'NONE',  ( -12.03266363877000167, 15.14665849299999856, -1.476125921680999875 ) ) ;
#15713 = CARTESIAN_POINT ( 'NONE',  ( 12.00000000000000000, -8.391897884961000642, -3.194141202603999918 ) ) ;
#15714 = CARTESIAN_POINT ( 'NONE',  ( 12.59887625730999972, 2.316137192978999781, 8.804988873405999783 ) ) ;
#15715 = ADVANCED_FACE ( 'NONE', ( #10240 ), #13013, .T. ) ;
#15716 = CARTESIAN_POINT ( 'NONE',  ( 2.184465970885649977, 27.53333333333333499, 1.259047450927240686 ) ) ;
#15717 = VERTEX_POINT ( 'NONE', #10118 ) ;
#15718 = CARTESIAN_POINT ( 'NONE',  ( 22.66677564524290744, 35.31760589360604996, 6.000000000000000000 ) ) ;
#15719 = CARTESIAN_POINT ( 'NONE',  ( -1.534530130794999891, 30.23743619718000275, -2.015030406789999784 ) ) ;
#15720 = AXIS2_PLACEMENT_3D ( 'NONE', #17761, #1164, #8558 ) ;
#15721 = DIRECTION ( 'NONE',  ( 0.000000000000000000, -1.000000000000000000, 0.000000000000000000 ) ) ;
#15722 = CARTESIAN_POINT ( 'NONE',  ( -2.281730950380269185, 13.94578545768103872, -5.684389550665945201 ) ) ;
#15723 = EDGE_LOOP ( 'NONE', ( #4114, #17358, #14783, #12811 ) ) ;
#15724 = AXIS2_PLACEMENT_3D ( 'NONE', #2140, #18620, #7231 ) ;
#15725 = CARTESIAN_POINT ( 'NONE',  ( 4.901867555465002191, 14.36018495061998657, -3.565049704023001365 ) ) ;
#15726 = FACE_OUTER_BOUND ( 'NONE', #18006, .T. ) ;
#15727 = ADVANCED_FACE ( 'NONE', ( #21503 ), #23057, .F. ) ;
#15728 = CARTESIAN_POINT ( 'NONE',  ( -2.745296661449999842, 28.97628422304000040, 0.04506516330758999350 ) ) ;
#15729 = CARTESIAN_POINT ( 'NONE',  ( 4.000000000000000000, 28.00000000000000000, -2.309401076759000304 ) ) ;
#15730 = B_SPLINE_CURVE_WITH_KNOTS ( 'NONE', 3,
 ( #12685, #23584, #22116, #1894, #23693, #20073, #3488, #21656, #10634, #8934, #23929, #12452, #12799, #21883, #9284, #6988, #1774, #16658, #3372, #5294, #7338, #9044, #1422, #8822, #21771, #5523, #16538, #16416, #62, #14719, #5183, #7101, #12902, #23806, #10868, #22001, #12565, #3248, #18021, #19835, #20302, #7214, #18362, #19953, #14491, #14377, #18253, #10750, #3704, #5414, #20186, #18145, #3596, #1548, #10979, #16302, #11097, #6446, #11225, #4281, #15637, #2827, #22789, #5635, #9962, #6324, #10089, #17475, #20985, #15400, #17349, #9395, #625, #16767, #9844, #753, #869, #6204, #15520, #18604, #19161, #4396, #4517, #2010, #8273, #175, #17225, #23029, #8155, #11787, #13832, #12032, #8026, #7567, #13589, #10207, #21233, #22908, #4645, #19415, #17601, #7448, #14946, #2705, #13709, #22341, #21104, #14828, #2573, #11908, #6078 ),
 .UNSPECIFIED., .F., .F.,
 ( 4, 2, 2, 2, 2, 2, 1, 2, 2, 2, 2, 2, 2, 2, 2, 2, 2, 2, 2, 2, 2, 2, 2, 2, 2, 2, 2, 2, 1, 2, 2, 2, 2, 2, 2, 2, 2, 2, 2, 2, 2, 2, 2, 2, 2, 2, 2, 2, 2, 2, 1, 2, 2, 2, 2, 2, 4 ),
 ( 0.000000000000000000, 0.01562500000000000000, 0.03125000000000000000, 0.04687500000000000694, 0.06250000000000001388, 0.07812500000000002776, 0.09375000000000004163, 0.1093750000000000555, 0.1250000000000000555, 0.1406250000000000555, 0.1562500000000000555, 0.1718750000000000555, 0.1875000000000000555, 0.2031250000000000555, 0.2187500000000000555, 0.2343750000000000555, 0.2500000000000000555, 0.2656250000000000555, 0.2812500000000000555, 0.2968750000000000555, 0.3125000000000000555, 0.3281250000000000555, 0.3437500000000000555, 0.3593750000000000555, 0.3750000000000000555, 0.4062500000000000555, 0.4375000000000000555, 0.4687500000000000555, 0.5000000000000001110, 0.5312500000000001110, 0.5625000000000001110, 0.5937500000000001110, 0.6250000000000001110, 0.6406250000000001110, 0.6562500000000001110, 0.6718750000000001110, 0.6875000000000001110, 0.7031250000000001110, 0.7187500000000001110, 0.7343750000000001110, 0.7500000000000001110, 0.7656250000000001110, 0.7812500000000001110, 0.7968750000000001110, 0.8125000000000001110, 0.8281250000000001110, 0.8437500000000001110, 0.8593750000000001110, 0.8750000000000001110, 0.8906250000000001110, 0.9062500000000001110, 0.9218750000000001110, 0.9375000000000001110, 0.9531250000000001110, 0.9687500000000001110, 0.9843750000000001110, 1.000000000000000000 ),
 .UNSPECIFIED. ) ;
#15731 = CARTESIAN_POINT ( 'NONE',  ( 15.06119984603782491, 3.964601025465794404, 9.748577488744984976 ) ) ;
#15732 = B_SPLINE_CURVE_WITH_KNOTS ( 'NONE', 3,
 ( #19885, #16241, #10565, #3423, #16354, #1477 ),
 .UNSPECIFIED., .F., .F.,
 ( 4, 2, 4 ),
 ( 0.000000000000000000, 0.5000000000000000000, 1.000000000000000000 ),
 .UNSPECIFIED. ) ;
#15733 = AXIS2_PLACEMENT_3D ( 'NONE', #10758, #18258, #21889 ) ;
#15734 = CARTESIAN_POINT ( 'NONE',  ( -14.25699038479000080, -13.93375672974000068, 0.1440191439639999793 ) ) ;
#15735 = DIRECTION ( 'NONE',  ( 0.000000000000000000, -1.000000000000000000, 0.000000000000000000 ) ) ;
#15736 = CARTESIAN_POINT ( 'NONE',  ( -24.17970357210941756, -8.771272208539420134, 9.807700027330906067 ) ) ;
#15737 = EDGE_LOOP ( 'NONE', ( #12917, #14989, #10947, #22103 ) ) ;
#15738 = CARTESIAN_POINT ( 'NONE',  ( -24.50000000000000711, -8.967281873253046598, -5.478788448042904768 ) ) ;
#15739 = CARTESIAN_POINT ( 'NONE',  ( 1.472141380057878868, 24.50000000000001421, -1.988599837602683218 ) ) ;
#15740 = EDGE_LOOP ( 'NONE', ( #23260, #22320, #19705, #15850 ) ) ;
#15741 = CARTESIAN_POINT ( 'NONE',  ( 2.112965035456999985, 25.89200715711999834, -0.7396727963457000454 ) ) ;
#15742 = CARTESIAN_POINT ( 'NONE',  ( -1.568717858167619994, 23.70514940564993012, -1.532321819884336023 ) ) ;
#15743 = EDGE_CURVE ( 'NONE', #14425, #3901, #11867, .T. ) ;
#15744 = CARTESIAN_POINT ( 'NONE',  ( 2.606584289605573979, 13.03356560933178976, 6.201593128633253293 ) ) ;
#15745 = VECTOR ( 'NONE', #13275, 1000.000000000000000 ) ;
#15746 = CARTESIAN_POINT ( 'NONE',  ( 6.144426515170381187, 14.17071861772576646, -0.1469360130798122999 ) ) ;
#15747 = CARTESIAN_POINT ( 'NONE',  ( -20.28383807595834298, -8.298568892495806537, 4.095387357305202869 ) ) ;
#15748 = CARTESIAN_POINT ( 'NONE',  ( 24.37173283531060264, -3.055078579629052271, -12.50000000000000000 ) ) ;
#15749 = AXIS2_PLACEMENT_3D ( 'NONE', #22603, #4206, #11600 ) ;
#15750 = ORIENTED_EDGE ( 'NONE', *, *, #23836, .T. ) ;
#15751 = DIRECTION ( 'NONE',  ( 0.000000000000000000, 0.000000000000000000, 1.000000000000000000 ) ) ;
#15752 = CARTESIAN_POINT ( 'NONE',  ( -1.103481847858666542, 6.865278473733852138, -1.376819519320963137 ) ) ;
#15753 = FACE_OUTER_BOUND ( 'NONE', #19682, .T. ) ;
#15754 = VERTEX_POINT ( 'NONE', #8552 ) ;
#15755 = CARTESIAN_POINT ( 'NONE',  ( -22.66095672860999954, -10.66205312073000044, -1.334338195151000273 ) ) ;
#15756 = DIRECTION ( 'NONE',  ( 1.552013396384999864E-11, 0.000000000000000000, 1.000000000000000000 ) ) ;
#15757 = CARTESIAN_POINT ( 'NONE',  ( 20.79345833333331939, 5.656740788837752554, -7.360929357356189584 ) ) ;
#15758 = CARTESIAN_POINT ( 'NONE',  ( 14.97266585189538368, 10.13449242591069144, 2.012324330117317039 ) ) ;
#15759 = CARTESIAN_POINT ( 'NONE',  ( -17.47543258502999919, -9.736197399936997954, -5.302291535354000551 ) ) ;
#15760 = EDGE_CURVE ( 'NONE', #8569, #17905, #10589, .T. ) ;
#15761 = LINE ( 'NONE', #13955, #7267 ) ;
#15762 = CARTESIAN_POINT ( 'NONE',  ( -22.86732996308985122, 4.662680996433341996, 8.088179580956165182 ) ) ;
#15763 = EDGE_CURVE ( 'NONE', #1014, #13308, #17755, .T. ) ;
#15764 = CARTESIAN_POINT ( 'NONE',  ( -1.406371714024999164, 11.64204510379998680, -4.531569040216001376 ) ) ;
#15765 = AXIS2_PLACEMENT_3D ( 'NONE', #13911, #664, #8070 ) ;
#15766 = CARTESIAN_POINT ( 'NONE',  ( 0.000000000000000000, 22.00000000000000000, 0.000000000000000000 ) ) ;
#15767 = CARTESIAN_POINT ( 'NONE',  ( -1.745680696064461523, 29.32358447642451438, -1.273442031135304964 ) ) ;
#15768 = EDGE_LOOP ( 'NONE', ( #16607, #5172, #10258, #11263 ) ) ;
#15769 = B_SPLINE_CURVE_WITH_KNOTS ( 'NONE', 3,
 ( #5596, #7769, #1965, #15137, #22534, #9349, #18908, #5940, #14905, #15025, #7522, #7653 ),
 .UNSPECIFIED., .F., .F.,
 ( 4, 1, 1, 1, 1, 2, 2, 4 ),
 ( 0.000000000000000000, 0.2500000000000041633, 0.3750000000000059952, 0.4375000000000063838, 0.4687500000000064948, 0.4843750000000064393, 0.5000000000000064393, 1.000000000000000000 ),
 .UNSPECIFIED. ) ;
#15770 = PLANE ( 'NONE',  #1047 ) ;
#15771 = CARTESIAN_POINT ( 'NONE',  ( -15.96785171052174412, -9.249139021331371779, 4.747086489963850298 ) ) ;
#15772 = ORIENTED_EDGE ( 'NONE', *, *, #436, .F. ) ;
#15773 = DIRECTION ( 'NONE',  ( 0.7071067811867980391, 0.7071067811862969954, -5.435108384955979519E-09 ) ) ;
#15774 = CARTESIAN_POINT ( 'NONE',  ( 5.066445834236000145, 14.82876933804001318, -3.462109428241999520 ) ) ;
#15775 = EDGE_CURVE ( 'NONE', #7466, #12844, #2992, .T. ) ;
#15776 = LINE ( 'NONE', #4897, #11949 ) ;
#15777 = EDGE_CURVE ( 'NONE', #5775, #8671, #20404, .T. ) ;
#15778 = CARTESIAN_POINT ( 'NONE',  ( 1.699999999999999956, 9.029776245285399128, -0.9151600407964531891 ) ) ;
#15779 = CARTESIAN_POINT ( 'NONE',  ( 14.38031392131000175, 9.076879665875999592, 3.306787424407999776 ) ) ;
#15780 = ORIENTED_EDGE ( 'NONE', *, *, #2004, .F. ) ;
#15781 = CARTESIAN_POINT ( 'NONE',  ( 23.99062354302999722, 7.716878364870000340, -11.63397459621999985 ) ) ;
#15782 = CIRCLE ( 'NONE', #13466, 2.673746900119611247 ) ;
#15783 = CARTESIAN_POINT ( 'NONE',  ( 0.000000000000000000, 18.00000000000000000, 0.000000000000000000 ) ) ;
#15784 = FILL_AREA_STYLE ('',( #19434 ) ) ;
#15785 = ORIENTED_EDGE ( 'NONE', *, *, #17552, .F. ) ;
#15786 = DIRECTION ( 'NONE',  ( 0.000000000000000000, 0.000000000000000000, -1.000000000000000000 ) ) ;
#15787 = FACE_OUTER_BOUND ( 'NONE', #23033, .T. ) ;
#15788 = CARTESIAN_POINT ( 'NONE',  ( -4.000000000000000000, 26.20000000000000284, 2.309401076759000304 ) ) ;
#15789 = CARTESIAN_POINT ( 'NONE',  ( 16.43228481845074640, 5.324967529146916512, -8.918705523749617115 ) ) ;
#15790 = CARTESIAN_POINT ( 'NONE',  ( 1.709999999999999964, 12.37689379448999993, -0.3720215047547999476 ) ) ;
#15791 = CONICAL_SURFACE ( 'NONE', #5365, 4.309401076758999416, 1.119376321708719590 ) ;
#15792 = CARTESIAN_POINT ( 'NONE',  ( -14.41332696916413170, -9.018101604870846444, 9.380024591087758878 ) ) ;
#15793 = CARTESIAN_POINT ( 'NONE',  ( 21.88640382367999848, 10.36782067078999958, -4.349542176122999315 ) ) ;
#15794 = CARTESIAN_POINT ( 'NONE',  ( -4.820913537080000033, 13.20111002679000123, 5.836439296936000609 ) ) ;
#15795 = VECTOR ( 'NONE', #2159, 1000.000000000000000 ) ;
#15796 = CARTESIAN_POINT ( 'NONE',  ( -4.267402886712965859, 13.63170725869960087, -4.942444299606017388 ) ) ;
#15797 = CARTESIAN_POINT ( 'NONE',  ( -2.098716048264661183, 30.17350835825882882, -0.5109231943707897017 ) ) ;
#15798 = ORIENTED_EDGE ( 'NONE', *, *, #14323, .F. ) ;
#15799 = CARTESIAN_POINT ( 'NONE',  ( 22.98509940575999977, -5.647570509607000133, -9.363978333943000720 ) ) ;
#15800 = CARTESIAN_POINT ( 'NONE',  ( 23.93104224056287777, 10.41832666982863564, -2.042517780468533051 ) ) ;
#15801 = CARTESIAN_POINT ( 'NONE',  ( 6.243179582884000212, 1.148189900220999940E-14, 0.000000000000000000 ) ) ;
#15802 = FACE_OUTER_BOUND ( 'NONE', #15152, .T. ) ;
#15803 = DIRECTION ( 'NONE',  ( 1.000000000000000000, 0.000000000000000000, 0.000000000000000000 ) ) ;
#15804 = CARTESIAN_POINT ( 'NONE',  ( -12.25000000000000000, -15.43375672973998824, 0.000000000000000000 ) ) ;
#15805 = ORIENTED_EDGE ( 'NONE', *, *, #20442, .F. ) ;
#15806 = AXIS2_PLACEMENT_3D ( 'NONE', #21077, #20960, #4488 ) ;
#15807 = CARTESIAN_POINT ( 'NONE',  ( 1.640193969998194001, 24.74015355458762144, 1.405240085690787843 ) ) ;
#15808 = DIRECTION ( 'NONE',  ( 0.000000000000000000, -1.000000000000000000, 0.000000000000000000 ) ) ;
#15809 = CONICAL_SURFACE ( 'NONE', #8484, 4.309401076758999416, 1.119376321708719590 ) ;
#15810 = CARTESIAN_POINT ( 'NONE',  ( 0.5508124349485069571, 27.39697001148643807, -2.099160625523386781 ) ) ;
#15811 = DIRECTION ( 'NONE',  ( 1.000000000000000000, 0.000000000000000000, 0.000000000000000000 ) ) ;
#15812 = DIRECTION ( 'NONE',  ( -0.000000000000000000, -1.000000000000000000, -0.000000000000000000 ) ) ;
#15813 = ORIENTED_EDGE ( 'NONE', *, *, #21985, .T. ) ;
#15814 = CARTESIAN_POINT ( 'NONE',  ( -10.04281598263999875, 16.40330333354999937, -1.000000000000000000 ) ) ;
#15815 = CONICAL_SURFACE ( 'NONE', #15432, 2.849999992212000066, 0.7853981633972997312 ) ;
#15816 = FACE_OUTER_BOUND ( 'NONE', #3261, .T. ) ;
#15817 = CARTESIAN_POINT ( 'NONE',  ( -14.47288607055999243, -6.205759095609786336, -6.641949884944085447 ) ) ;
#15818 = CARTESIAN_POINT ( 'NONE',  ( -13.80102035161000096, -0.9449678463817999807, -10.71550788283000166 ) ) ;
#15819 = CARTESIAN_POINT ( 'NONE',  ( -6.306081500775003512, 16.13779117371002059, 0.9717814567668997539 ) ) ;
#15820 = CARTESIAN_POINT ( 'NONE',  ( 18.64619494525999954, 2.446936341558000105, -10.06727026104000089 ) ) ;
#15821 = CARTESIAN_POINT ( 'NONE',  ( 1.852496879401591912, 28.27448153086328730, -1.136612110235776019 ) ) ;
#15822 = CARTESIAN_POINT ( 'NONE',  ( -24.50000000000000000, -8.081477262649000792, -6.807253044743999837 ) ) ;
#15823 = TOROIDAL_SURFACE ( 'NONE', #5401, 16.43375672870000059, 1.000000000000000000 ) ;
#15824 = CARTESIAN_POINT ( 'NONE',  ( 0.000000000000000000, 21.89999999999999858, -4.749999999999985789 ) ) ;
#15825 = EDGE_LOOP ( 'NONE', ( #15081, #14335 ) ) ;
#15826 = CARTESIAN_POINT ( 'NONE',  ( 2.504532394112000003E-14, 28.43419673618999965, 2.500000000000000000 ) ) ;
#15827 = CARTESIAN_POINT ( 'NONE',  ( 1.834054417453000019, 26.46369850838000204, 1.332518472557000067 ) ) ;
#15828 = CIRCLE ( 'NONE', #22400, 2.750000000000000000 ) ;
#15829 = CIRCLE ( 'NONE', #13122, 2.948682383037074750 ) ;
#15830 = FACE_OUTER_BOUND ( 'NONE', #3525, .T. ) ;
#15831 = CARTESIAN_POINT ( 'NONE',  ( -14.52843611649297806, 0.8125160302300082904, -9.009207629665930028 ) ) ;
#15832 = CARTESIAN_POINT ( 'NONE',  ( -19.59647822760999958, -9.324997552198999173, 5.908885382590000290 ) ) ;
#15833 = CARTESIAN_POINT ( 'NONE',  ( -8.099999999999999645, 1.323843189878000027E-14, 0.000000000000000000 ) ) ;
#15834 = ORIENTED_EDGE ( 'NONE', *, *, #5231, .T. ) ;
#15835 = CARTESIAN_POINT ( 'NONE',  ( 3.161491510400058047, 11.90317520361505821, -3.649523268417677713 ) ) ;
#15836 = CARTESIAN_POINT ( 'NONE',  ( 4.901795610954997606, 14.36014350025000219, 3.565170190326997446 ) ) ;
#15837 = CARTESIAN_POINT ( 'NONE',  ( 1.283659224277774236, 6.897942598336115338, 1.193638655190912168 ) ) ;
#15838 = DIRECTION ( 'NONE',  ( 0.4226182617406808451, 0.000000000000000000, -0.9063077870366587074 ) ) ;
#15839 = EDGE_CURVE ( 'NONE', #19206, #3147, #7224, .T. ) ;
#15840 = CARTESIAN_POINT ( 'NONE',  ( -2.434931691670790155, 27.40086340285667532, -0.6543697108981963995 ) ) ;
#15841 = CARTESIAN_POINT ( 'NONE',  ( -16.08338753829999845, -2.146827734392999787, 11.15102392286999944 ) ) ;
#15842 = CARTESIAN_POINT ( 'NONE',  ( 11.31918875731000007, -8.923818741964000267, -0.1967739533420000131 ) ) ;
#15843 = CARTESIAN_POINT ( 'NONE',  ( 24.43449445986659896, 2.200516184495611594, 12.50000000000000000 ) ) ;
#15844 = ORIENTED_EDGE ( 'NONE', *, *, #16060, .F. ) ;
#15845 = CARTESIAN_POINT ( 'NONE',  ( 5.302309868036999774, 13.73032359673999814, 4.450989051274000019 ) ) ;
#15846 = CARTESIAN_POINT ( 'NONE',  ( -2.032503672545999951, 30.43597535861000125, 1.511310389916999952 ) ) ;
#15847 = CARTESIAN_POINT ( 'NONE',  ( 2.661087342023999547, 23.74853527822999766, 0.5436575690810000472 ) ) ;
#15848 = DIRECTION ( 'NONE',  ( 1.000000000000000000, 0.000000000000000000, 0.000000000000000000 ) ) ;
#15849 = CIRCLE ( 'NONE', #22425, 4.649999999999999467 ) ;
#15850 = ORIENTED_EDGE ( 'NONE', *, *, #18678, .T. ) ;
#15851 = DIRECTION ( 'NONE',  ( 1.000000000000000000, 0.000000000000000000, 0.000000000000000000 ) ) ;
#15852 = CARTESIAN_POINT ( 'NONE',  ( -24.43506354683006165, 11.72249354572300106, -4.696109227427953670 ) ) ;
#15853 = CARTESIAN_POINT ( 'NONE',  ( -2.344225979797000203, 28.90447533745000186, -1.429436635564000024 ) ) ;
#15854 = EDGE_CURVE ( 'NONE', #14047, #2155, #20615, .T. ) ;
#15855 = CARTESIAN_POINT ( 'NONE',  ( -23.71390419459027754, -9.377614579209383905, 1.734352417475094388 ) ) ;
#15856 = CARTESIAN_POINT ( 'NONE',  ( 16.62232292872420558, 9.925332452011865314, 3.188991502716413073 ) ) ;
#15857 = CARTESIAN_POINT ( 'NONE',  ( -4.000000000000000000, 24.80000000000000426, 2.309401076759000304 ) ) ;
#15858 = CARTESIAN_POINT ( 'NONE',  ( -21.66299577250665820, -4.646874200087295570, -8.062647617244037335 ) ) ;
#15859 = CARTESIAN_POINT ( 'NONE',  ( -24.41904027020013146, -9.801083277811052596, 8.024000954858145462 ) ) ;
#15860 = EDGE_LOOP ( 'NONE', ( #4078, #794, #2341, #20437 ) ) ;
#15861 = CARTESIAN_POINT ( 'NONE',  ( -24.50000000000000000, -9.826472200743234353, -3.257612521534738015 ) ) ;
#15862 = CARTESIAN_POINT ( 'NONE',  ( 11.06619116164413619, -11.07450388079853809, 5.818393174557106029 ) ) ;
#15863 = ORIENTED_EDGE ( 'NONE', *, *, #18962, .F. ) ;
#15864 = CARTESIAN_POINT ( 'NONE',  ( -0.7526554537551000124, 24.11634424051000281, 2.431350270797000057 ) ) ;
#15865 = DIRECTION ( 'NONE',  ( -1.000000000000000000, 0.000000000000000000, 0.000000000000000000 ) ) ;
#15866 = CARTESIAN_POINT ( 'NONE',  ( -2.918874744973449786, 13.09137196612760157, 6.078593498656847949 ) ) ;
#15867 = CARTESIAN_POINT ( 'NONE',  ( 12.51792910804999970, 13.93375672974000068, 0.7216190549664999176 ) ) ;
#15868 = FACE_OUTER_BOUND ( 'NONE', #15640, .T. ) ;
#15869 = EDGE_CURVE ( 'NONE', #7389, #837, #21092, .T. ) ;
#15870 = CARTESIAN_POINT ( 'NONE',  ( -6.042815837158999948, 16.37762238964999995, -0.9999999878869999526 ) ) ;
#15871 = EDGE_LOOP ( 'NONE', ( #23016, #21369, #20992, #17914 ) ) ;
#15872 = CARTESIAN_POINT ( 'NONE',  ( -12.41173981160000039, 6.613190111079999767, -13.46349570337000046 ) ) ;
#15873 = DIRECTION ( 'NONE',  ( 0.000000000000000000, 0.000000000000000000, 1.000000000000000000 ) ) ;
#15874 = DIRECTION ( 'NONE',  ( 0.000000000000000000, 1.000000000000000000, 0.000000000000000000 ) ) ;
#15875 = ORIENTED_EDGE ( 'NONE', *, *, #21380, .F. ) ;
#15876 = CARTESIAN_POINT ( 'NONE',  ( -21.56023462137999758, 10.17996857714999948, -0.5018336655562000148 ) ) ;
#15877 = CARTESIAN_POINT ( 'NONE',  ( -1.346439123299412177, 28.03198827073827459, -3.841100253456362523 ) ) ;
#15878 = CARTESIAN_POINT ( 'NONE',  ( 15.06027663792326265, 9.078858026381649182, 4.937948093896874724 ) ) ;
#15879 = DIRECTION ( 'NONE',  ( 1.000000000000000000, 0.000000000000000000, 0.000000000000000000 ) ) ;
#15880 = DIRECTION ( 'NONE',  ( 0.000000000000000000, 1.000000000000000000, 0.000000000000000000 ) ) ;
#15881 = EDGE_CURVE ( 'NONE', #11881, #8871, #9970, .T. ) ;
#15882 = CARTESIAN_POINT ( 'NONE',  ( 2.099999992529999915, 28.30000000747030242, 4.159306788217000353E-08 ) ) ;
#15883 = CARTESIAN_POINT ( 'NONE',  ( 4.148757769666998385, 12.31837238841998783, -2.295775157709002201 ) ) ;
#15884 = VERTEX_POINT ( 'NONE', #19528 ) ;
#15885 = CARTESIAN_POINT ( 'NONE',  ( -14.25521440656999950, -2.679375877985999743, 10.98274110836000084 ) ) ;
#15886 = CARTESIAN_POINT ( 'NONE',  ( -1.841895772823868960, 29.33354493891415160, -1.134390543764295822 ) ) ;
#15887 = ORIENTED_EDGE ( 'NONE', *, *, #3608, .F. ) ;
#15888 = CARTESIAN_POINT ( 'NONE',  ( 0.6543697108981982868, 29.36666666666666359, -2.434931691670790155 ) ) ;
#15889 = CARTESIAN_POINT ( 'NONE',  ( -15.15755484276677656, 7.261073034381060332, -7.630493215577654809 ) ) ;
#15890 = ADVANCED_FACE ( 'NONE', ( #1233 ), #23857, .F. ) ;
#15891 = VERTEX_POINT ( 'NONE', #8623 ) ;
#15892 = CARTESIAN_POINT ( 'NONE',  ( 6.461460758271004856, 13.53984578379000325, -1.553565135251000484 ) ) ;
#15893 = CARTESIAN_POINT ( 'NONE',  ( 12.00000000000000000, -3.698948358382036172, -8.182095219967926880 ) ) ;
#15894 = ADVANCED_FACE ( 'NONE', ( #12023 ), #17346, .F. ) ;
#15895 = CARTESIAN_POINT ( 'NONE',  ( 15.17456408531000100, -6.393444021559000490, 7.935320769223000781 ) ) ;
#15896 = ADVANCED_FACE ( 'NONE', ( #17714 ), #1110, .F. ) ;
#15897 = ORIENTED_EDGE ( 'NONE', *, *, #5144, .F. ) ;
#15898 = DIRECTION ( 'NONE',  ( 0.8866244295713172630, 0.000000000000000000, 0.4624901305837091359 ) ) ;
#15899 = CARTESIAN_POINT ( 'NONE',  ( 1.259047450927246903, 26.93333333333332646, -2.184465970885645536 ) ) ;
#15900 = CARTESIAN_POINT ( 'NONE',  ( 2.327192509895192885, 24.50639765414752702, -3.274853329251975698 ) ) ;
#15901 = ORIENTED_EDGE ( 'NONE', *, *, #17390, .T. ) ;
#15902 = CARTESIAN_POINT ( 'NONE',  ( -5.730762473771000565, 26.50000000000000000, 1.577381738259000077 ) ) ;
#15903 = DIRECTION ( 'NONE',  ( -0.000000000000000000, -1.000000000000000000, -0.000000000000000000 ) ) ;
#15904 = CARTESIAN_POINT ( 'NONE',  ( -2.160826008357635164, 26.50000000000000355, 3.371248675920325955 ) ) ;
#15905 = CARTESIAN_POINT ( 'NONE',  ( 16.39583361425184549, 4.159787878704626074, -9.519236833959350719 ) ) ;
#15906 = CARTESIAN_POINT ( 'NONE',  ( -16.27887281610000159, 9.774068015792000352, 5.162340849467000226 ) ) ;
#15907 = CARTESIAN_POINT ( 'NONE',  ( -14.47826291725376358, -11.73192043637804893, 4.679722760534371417 ) ) ;
#15908 = EDGE_CURVE ( 'NONE', #3069, #2709, #19811, .T. ) ;
#15909 = EDGE_CURVE ( 'NONE', #6758, #16136, #14319, .T. ) ;
#15910 = CARTESIAN_POINT ( 'NONE',  ( 1.595510613210902928, 26.49040384242091761, 3.697633671484740425 ) ) ;
#15911 = CARTESIAN_POINT ( 'NONE',  ( -2.080319161808850570, 30.16916080325708904, -0.5827450134709621921 ) ) ;
#15912 = ORIENTED_EDGE ( 'NONE', *, *, #12322, .F. ) ;
#15913 = CARTESIAN_POINT ( 'NONE',  ( -24.11803009774280326, -4.367939700960269178, 12.49970390894446659 ) ) ;
#15914 = CARTESIAN_POINT ( 'NONE',  ( 22.21209567152000020, 0.8567587614818000796, 10.88017005124000036 ) ) ;
#15915 = CARTESIAN_POINT ( 'NONE',  ( 0.000000000000000000, 17.00000000000000000, -2.704938617610999654E-14 ) ) ;
#15916 = CARTESIAN_POINT ( 'NONE',  ( -1.605639779780836829, 23.61395945400231611, -1.383350294238146372 ) ) ;
#15917 = ORIENTED_EDGE ( 'NONE', *, *, #15295, .T. ) ;
#15918 = CYLINDRICAL_SURFACE ( 'NONE', #11842, 10.59999999999999964 ) ;
#15919 = CARTESIAN_POINT ( 'NONE',  ( -3.100000000000000089, 22.00000000000000000, 0.000000000000000000 ) ) ;
#15920 = CARTESIAN_POINT ( 'NONE',  ( 4.913254300577998279, 12.43880135910001172, 0.1079351427945999670 ) ) ;
#15921 = ORIENTED_EDGE ( 'NONE', *, *, #4312, .F. ) ;
#15922 = CARTESIAN_POINT ( 'NONE',  ( -15.45146194107333493, -8.546491615899846295, -6.146800611315578422 ) ) ;
#15923 = CIRCLE ( 'NONE', #7039, 2.100000000000000089 ) ;
#15924 = CARTESIAN_POINT ( 'NONE',  ( 17.97356375731000000, 4.354347264933000616, 8.156255255558999551 ) ) ;
#15925 = VERTEX_POINT ( 'NONE', #12391 ) ;
#15926 = CARTESIAN_POINT ( 'NONE',  ( -0.8667355603187372193, 26.97782460062819254, 2.020380412232955170 ) ) ;
#15927 = DIRECTION ( 'NONE',  ( -1.000000000000000000, 0.000000000000000000, 0.000000000000000000 ) ) ;
#15928 = ORIENTED_EDGE ( 'NONE', *, *, #13055, .T. ) ;
#15929 = DIRECTION ( 'NONE',  ( 0.8500000000000165201, 0.000000000000000000, -0.5267826876426102700 ) ) ;
#15930 = CARTESIAN_POINT ( 'NONE',  ( -12.40106293735999898, 6.430159825535999296, -13.55186498671000095 ) ) ;
#15931 = CARTESIAN_POINT ( 'NONE',  ( -14.41377531173998960, -4.730461704047363547, -7.760299280567290126 ) ) ;
#15932 = CARTESIAN_POINT ( 'NONE',  ( -18.87927905085999924, 10.04277392903999910, -4.232445057647000297 ) ) ;
#15934 = ADVANCED_FACE ( 'NONE', ( #6676, #14068 ), #18072, .T. ) ;
#15933 = DIRECTION ( 'NONE',  ( -0.5000000000000169864, 0.000000000000000000, -0.8660254037844289376 ) ) ;
#15935 = CARTESIAN_POINT ( 'NONE',  ( 18.44306994526000310, -4.644512059083999667, -9.254651726414000024 ) ) ;
#15936 = CARTESIAN_POINT ( 'NONE',  ( -4.000000000000000888, 26.37418302490047850, -1.506880184559495017 ) ) ;
#15937 = CARTESIAN_POINT ( 'NONE',  ( 2.000000000000000000, 26.50000000000000355, -3.464101615137999968 ) ) ;
#15938 = CARTESIAN_POINT ( 'NONE',  ( 15.46483333333333121, 7.923568558109999493, -4.567004612312420164 ) ) ;
#15939 = EDGE_LOOP ( 'NONE', ( #14798, #17858 ) ) ;
#15940 = CARTESIAN_POINT ( 'NONE',  ( -17.00872087121333109, -7.283262656812431679, 5.597053662224771742 ) ) ;
#15941 = CARTESIAN_POINT ( 'NONE',  ( -0.2992355516767008505, 13.69531868001229569, 6.118419485397218693 ) ) ;
#15942 = B_SPLINE_CURVE_WITH_KNOTS ( 'NONE', 3,
 ( #20236, #3755, #11143, #18529, #15940, #1310, #23811, #23459, #22007, #5421, #10639, #14497, #18151, #4951, #6750, #9050, #3139, #10523 ),
 .UNSPECIFIED., .F., .F.,
 ( 4, 2, 2, 2, 2, 2, 2, 2, 4 ),
 ( 0.000000000000000000, 0.1250000000000000278, 0.2500000000000000555, 0.3750000000000001110, 0.5000000000000000000, 0.6250000000000000000, 0.7500000000000000000, 0.8750000000000001110, 1.000000000000000000 ),
 .UNSPECIFIED. ) ;
#15943 = CARTESIAN_POINT ( 'NONE',  ( 1.994688225595000253, 25.78913313894999959, 1.016344414748000080 ) ) ;
#15944 = CIRCLE ( 'NONE', #17909, 4.649999999999999467 ) ;
#15945 = FACE_OUTER_BOUND ( 'NONE', #7974, .T. ) ;
#15946 = CARTESIAN_POINT ( 'NONE',  ( -14.40214030274523083, 4.602063563387535083, -7.815556307968948069 ) ) ;
#15947 = CARTESIAN_POINT ( 'NONE',  ( -19.63171012731000076, -10.46828650075000056, 1.869663484996999969 ) ) ;
#15948 = CARTESIAN_POINT ( 'NONE',  ( -3.938174484868301128, 12.12902309718726102, 2.809906632184955289 ) ) ;
#15949 = EDGE_LOOP ( 'NONE', ( #6945, #7664, #8684, #3085 ) ) ;
#15950 = DIRECTION ( 'NONE',  ( 1.000000000000000000, 0.000000000000000000, 0.000000000000000000 ) ) ;
#15951 = CARTESIAN_POINT ( 'NONE',  ( 3.092048582739372442, 11.88530494256604086, -3.707092650763546882 ) ) ;
#15952 = DIRECTION ( 'NONE',  ( 0.000000000000000000, 0.000000000000000000, -1.000000000000000000 ) ) ;
#15953 = CARTESIAN_POINT ( 'NONE',  ( 12.00000000000000000, 5.273090321616999532, -7.267806174758000282 ) ) ;
#15954 = CARTESIAN_POINT ( 'NONE',  ( 0.000000000000000000, 9.050044887908999414, 0.000000000000000000 ) ) ;
#15955 = CARTESIAN_POINT ( 'NONE',  ( -8.035714285714000482, -9.574826156038998448, 0.000000000000000000 ) ) ;
#15956 = CIRCLE ( 'NONE', #5532, 2.000000000000000000 ) ;
#15957 = CARTESIAN_POINT ( 'NONE',  ( 17.45156392131000089, -0.08049851871593999286, -9.740865876825999692 ) ) ;
#15958 = CARTESIAN_POINT ( 'NONE',  ( 0.000000000000000000, 17.00000000000000000, 0.000000000000000000 ) ) ;
#15959 = ORIENTED_EDGE ( 'NONE', *, *, #7583, .T. ) ;
#15960 = CARTESIAN_POINT ( 'NONE',  ( -22.21032711986755004, -6.106567764693699552, 6.962914243618090637 ) ) ;
#15961 = CARTESIAN_POINT ( 'NONE',  ( -1.747945498421000110, 29.54871418206000300, -2.089014728103999907 ) ) ;
#15962 = CARTESIAN_POINT ( 'NONE',  ( -14.97387077250666820, -5.565142630449472883, 7.241325911418540429 ) ) ;
#15963 = CARTESIAN_POINT ( 'NONE',  ( 4.027454389662117329, 14.47011947778932850, -4.614682357420342385 ) ) ;
#15964 = ORIENTED_EDGE ( 'NONE', *, *, #18692, .F. ) ;
#15965 = DIRECTION ( 'NONE',  ( 1.000000000000000000, 0.000000000000000000, 0.000000000000000000 ) ) ;
#15966 = CARTESIAN_POINT ( 'NONE',  ( 8.837430739852999650, 1.116419486464999937E-14, 0.000000000000000000 ) ) ;
#15967 = CARTESIAN_POINT ( 'NONE',  ( 6.124879597941472298, 14.37505545965193399, 0.1297071231249629641 ) ) ;
#15968 = DIRECTION ( 'NONE',  ( 0.5000000000000169864, 0.000000000000000000, -0.8660254037844288266 ) ) ;
#15969 = CARTESIAN_POINT ( 'NONE',  ( -4.105614703109887742, 13.75508681659879784, 4.877901297121352897 ) ) ;
#15970 = CARTESIAN_POINT ( 'NONE',  ( -4.351728331912002368, 12.23318868280000338, 2.300835253139998038 ) ) ;
#15971 = ADVANCED_FACE ( 'NONE', ( #17588 ), #983, .T. ) ;
#15972 = DIRECTION ( 'NONE',  ( 0.000000000000000000, -1.000000000000000000, 0.000000000000000000 ) ) ;
#15973 = ORIENTED_EDGE ( 'NONE', *, *, #4818, .F. ) ;
#15974 = CARTESIAN_POINT ( 'NONE',  ( 0.000000000000000000, 24.80000000000000426, 4.618802153517000519 ) ) ;
#15975 = PRODUCT_DEFINITION_FORMATION_WITH_SPECIFIED_SOURCE ( 'ANY', '', #13851, .NOT_KNOWN. ) ;
#15976 = CARTESIAN_POINT ( 'NONE',  ( 1.317056079378642108, 23.81658996185279875, 1.926182033697757534 ) ) ;
#15977 = EDGE_LOOP ( 'NONE', ( #15601, #17647 ) ) ;
#15978 = CARTESIAN_POINT ( 'NONE',  ( -1.734000915526999975, 25.54365575949000089, 1.590878194398000156 ) ) ;
#15979 = CARTESIAN_POINT ( 'NONE',  ( 23.41677564524290744, 34.01856778792605240, -6.000000000000005329 ) ) ;
#15980 = CARTESIAN_POINT ( 'NONE',  ( -3.018886224429293552, 13.11113671311871265, 6.035875662628554572 ) ) ;
#15981 = CARTESIAN_POINT ( 'NONE',  ( 0.000000000000000000, 28.15000000000000213, 0.000000000000000000 ) ) ;
#15982 = CARTESIAN_POINT ( 'NONE',  ( -5.737494891779999939, 16.36109002579999228, -2.188889223574999487 ) ) ;
#15983 = CONICAL_SURFACE ( 'NONE', #5922, 3.049999825846000157, 0.7853981633972997312 ) ;
#15984 = CARTESIAN_POINT ( 'NONE',  ( -16.81976253787999909, -9.102909969768001375, 0.000000000000000000 ) ) ;
#15985 = EDGE_CURVE ( 'NONE', #19406, #20779, #4227, .T. ) ;
#15986 = ORIENTED_EDGE ( 'NONE', *, *, #19133, .T. ) ;
#15987 = CARTESIAN_POINT ( 'NONE',  ( -0.3272492347489284192, 30.01753006952332825, 2.500000000000001332 ) ) ;
#15988 = DIRECTION ( 'NONE',  ( 0.9967542221350019771, 0.000000000000000000, 0.08050478654122018851 ) ) ;
#15989 = CARTESIAN_POINT ( 'NONE',  ( -14.00000000000000000, -10.59999999999999964, 0.000000000000000000 ) ) ;
#15990 = VERTEX_POINT ( 'NONE', #23745 ) ;
#15991 = CARTESIAN_POINT ( 'NONE',  ( -19.91908895889000064, 10.46467446202999874, 2.086251744724999746 ) ) ;
#15992 = DIRECTION ( 'NONE',  ( 1.000000000000000000, 0.000000000000000000, 0.000000000000000000 ) ) ;
#15993 = CARTESIAN_POINT ( 'NONE',  ( 15.23439172698186006, 4.645476851500599302, 9.236356228214244624 ) ) ;
#15994 = DIRECTION ( 'NONE',  ( 0.000000000000000000, -1.000000000000000000, 0.000000000000000000 ) ) ;
#15995 = CARTESIAN_POINT ( 'NONE',  ( 0.2973205334010999845, 29.50801477156000274, 2.147506602161000089 ) ) ;
#15996 = DIRECTION ( 'NONE',  ( 0.000000000000000000, 0.000000000000000000, -1.000000000000000000 ) ) ;
#15997 = CARTESIAN_POINT ( 'NONE',  ( -4.089491575493999775, 12.29838637034998428, -2.375562731294997842 ) ) ;
#15998 = VERTEX_POINT ( 'NONE', #11031 ) ;
#15999 = CARTESIAN_POINT ( 'NONE',  ( -16.48964823424000059, 10.66299948276999920, 3.938515806081000825 ) ) ;
#16000 = ADVANCED_FACE ( 'NONE', ( #21820 ), #18415, .T. ) ;
#16001 = CARTESIAN_POINT ( 'NONE',  ( 1.568686367319726882, 29.10097142498572964, -1.495817114762474809 ) ) ;
#16002 = ORIENTED_EDGE ( 'NONE', *, *, #13261, .F. ) ;
#16003 = AXIS2_PLACEMENT_3D ( 'NONE', #16359, #21935, #14428 ) ;
#16004 = CARTESIAN_POINT ( 'NONE',  ( -2.434931691670790155, 29.56666666666666288, -0.6543697108981958444 ) ) ;
#16005 = CARTESIAN_POINT ( 'NONE',  ( -14.89710227813126231, 10.31717450065112196, 0.9898032812542618686 ) ) ;
#16006 = VERTEX_POINT ( 'NONE', #14658 ) ;
#16007 = CARTESIAN_POINT ( 'NONE',  ( -1.767766952966000060, 30.50000000000000000, 1.767766952966000060 ) ) ;
#16008 = CARTESIAN_POINT ( 'NONE',  ( 11.06626444616536453, -10.95085460510079578, -6.032555207299142630 ) ) ;
#16009 = CARTESIAN_POINT ( 'NONE',  ( 12.00000000000000533, -8.178800721840129739, -3.754006756144630419 ) ) ;
#16010 = CARTESIAN_POINT ( 'NONE',  ( 24.36414987671881605, 3.145589772713091481, -12.50000000000000178 ) ) ;
#16011 = EDGE_CURVE ( 'NONE', #3493, #1813, #8116, .T. ) ;
#16012 = CARTESIAN_POINT ( 'NONE',  ( 15.39393908531000044, -10.10652924631000005, 1.349470982713999900 ) ) ;
#16013 = ORIENTED_EDGE ( 'NONE', *, *, #18856, .F. ) ;
#16014 = CARTESIAN_POINT ( 'NONE',  ( -10.41825149291999963, 4.409629518443999530, -13.83169641490000146 ) ) ;
#16015 = CARTESIAN_POINT ( 'NONE',  ( 13.49999999999999822, 9.585208429812723807, 0.5427004933114440988 ) ) ;
#16016 = CARTESIAN_POINT ( 'NONE',  ( 2.653270836322024984, 24.53198827073824617, -3.086600612158302948 ) ) ;
#16017 = VERTEX_POINT ( 'NONE', #3425 ) ;
#16018 = CARTESIAN_POINT ( 'NONE',  ( -23.54411375508000148, 0.8581424843098000022, -9.685395125838999419 ) ) ;
#16019 = FACE_OUTER_BOUND ( 'NONE', #10533, .T. ) ;
#16020 = CARTESIAN_POINT ( 'NONE',  ( 22.76464544783179278, -9.731360964096962718, 4.172095693800953242 ) ) ;
#16021 = FACE_OUTER_BOUND ( 'NONE', #9593, .T. ) ;
#16022 = CARTESIAN_POINT ( 'NONE',  ( 16.27409532413455651, -0.09483548955922246892, -10.36544530239856776 ) ) ;
#16023 = ADVANCED_FACE ( 'NONE', ( #18536 ), #17398, .F. ) ;
#16024 = CARTESIAN_POINT ( 'NONE',  ( -19.16948585659999793, -11.07481571228000128, 1.129444447747999902 ) ) ;
#16025 = CARTESIAN_POINT ( 'NONE',  ( 0.000000000000000000, 15.00000000000000000, 0.000000000000000000 ) ) ;
#16026 = CONICAL_SURFACE ( 'NONE', #5967, 13.20532192316000142, 0.7853981633972997312 ) ;
#16027 = CARTESIAN_POINT ( 'NONE',  ( -3.821786116376766795, 14.05616651468782408, -4.851985683239589342 ) ) ;
#16028 = ADVANCED_FACE ( 'NONE', ( #18304 ), #19691, .F. ) ;
#16029 = CARTESIAN_POINT ( 'NONE',  ( -2.155035702249775476, 30.21239445103314836, 0.1465990187513959708 ) ) ;
#16030 = ORIENTED_EDGE ( 'NONE', *, *, #19016, .T. ) ;
#16031 = B_SPLINE_CURVE_WITH_KNOTS ( 'NONE', 3,
 ( #19633, #14297, #2798, #17933 ),
 .UNSPECIFIED., .F., .F.,
 ( 4, 4 ),
 ( 0.000000000000000000, 1.000000000000000000 ),
 .UNSPECIFIED. ) ;
#16032 = CARTESIAN_POINT ( 'NONE',  ( 1.940244192847000004, 25.08955421093999760, -1.300335925705000006 ) ) ;
#16033 = CARTESIAN_POINT ( 'NONE',  ( 11.55284350193159781, 9.059841367859290173, -9.307687628695044069 ) ) ;
#16034 = B_SPLINE_CURVE_WITH_KNOTS ( 'NONE', 3,
 ( #5921, #23860, #16946, #18653, #3646, #11392, #14886, #5692, #2059, #14660 ),
 .UNSPECIFIED., .F., .F.,
 ( 4, 1, 1, 2, 2, 4 ),
 ( 0.000000000000000000, 0.2500000000000002776, 0.3750000000000006106, 0.4375000000000007216, 0.5000000000000009992, 1.000000000000000000 ),
 .UNSPECIFIED. ) ;
#16035 = CARTESIAN_POINT ( 'NONE',  ( 24.10128254254044222, 9.799474070031209294, 4.098014295304180266 ) ) ;
#16036 = CARTESIAN_POINT ( 'NONE',  ( -1.189123363982122816, 23.61714873636219636, -1.751662368594682162 ) ) ;
#16037 = CIRCLE ( 'NONE', #5603, 3.000000000000000000 ) ;
#16038 = ORIENTED_EDGE ( 'NONE', *, *, #10534, .T. ) ;
#16039 = FACE_OUTER_BOUND ( 'NONE', #6897, .T. ) ;
#16040 = CARTESIAN_POINT ( 'NONE',  ( -24.37124162822864903, -12.10385983559206657, -4.035505227296023456 ) ) ;
#16041 = CARTESIAN_POINT ( 'NONE',  ( 4.344185795461002364, 12.29657164613998965, -2.399808224106998455 ) ) ;
#16042 = ORIENTED_EDGE ( 'NONE', *, *, #6661, .F. ) ;
#16043 = CARTESIAN_POINT ( 'NONE',  ( -14.55830234973948301, 8.677646559420217898, 5.656680062773181916 ) ) ;
#16044 = ADVANCED_FACE ( 'NONE', ( #7265 ), #6095, .F. ) ;
#16045 = CARTESIAN_POINT ( 'NONE',  ( 17.86387625731000028, 7.066414026761999700, 5.957971218261000956 ) ) ;
#16046 = EDGE_LOOP ( 'NONE', ( #1621, #16109, #19313, #10092, #1126, #23249 ) ) ;
#16047 = CIRCLE ( 'NONE', #10661, 12.50000000000000178 ) ;
#16048 = CARTESIAN_POINT ( 'NONE',  ( 0.3732672031689003855, 27.05179143783847451, 2.138410171147020922 ) ) ;
#16049 = ITEM_DEFINED_TRANSFORMATION ( 'NONE', 'NONE', #2054,  #4390 ) ;
#16050 = CARTESIAN_POINT ( 'NONE',  ( -14.32799115069066964, -5.161629268668690429, -12.49976764740148738 ) ) ;
#16051 = VERTEX_POINT ( 'NONE', #2906 ) ;
#16052 = CARTESIAN_POINT ( 'NONE',  ( -19.20402730749667342, 3.634917981653388530, 8.480016702260009254 ) ) ;
#16053 = CARTESIAN_POINT ( 'NONE',  ( -4.488270148404611248, 15.47262777994140492, -4.168027791541332405 ) ) ;
#16054 = CARTESIAN_POINT ( 'NONE',  ( -22.34908598416999936, 4.767165090499999813, 8.950667383615998673 ) ) ;
#16055 = CARTESIAN_POINT ( 'NONE',  ( -17.92967774839999962, -8.030155173115000267, -6.508010117819000406 ) ) ;
#16056 = CARTESIAN_POINT ( 'NONE',  ( -1.888459278277104156E-11, 26.49469377355791977, -2.394693773557865057 ) ) ;
#16057 = CARTESIAN_POINT ( 'NONE',  ( 16.61494494526000310, -5.066514564376999097, -8.972071948347000614 ) ) ;
#16058 = CARTESIAN_POINT ( 'NONE',  ( 0.3219846793369715576, 27.58545158304634626, -2.185093432021212312 ) ) ;
#16059 = CARTESIAN_POINT ( 'NONE',  ( 20.23031853028999905, -9.645356037285999662, -0.7083642361915000185 ) ) ;
#16060 = EDGE_CURVE ( 'NONE', #11527, #13583, #9417, .T. ) ;
#16061 = DIRECTION ( 'NONE',  ( 0.000000000000000000, -1.000000000000000000, 0.000000000000000000 ) ) ;
#16062 = EDGE_LOOP ( 'NONE', ( #4316, #1369, #17762, #13539 ) ) ;
#16063 = EDGE_CURVE ( 'NONE', #5788, #20521, #8474, .T. ) ;
#16064 = CARTESIAN_POINT ( 'NONE',  ( 0.1602288781992032007, 13.69217011570514408, 6.122907753317686996 ) ) ;
#16065 = CARTESIAN_POINT ( 'NONE',  ( 1.745401010056999880, 27.34913313894999831, 1.745401010056999880 ) ) ;
#16066 = AXIS2_PLACEMENT_3D ( 'NONE', #6139, #22965, #6259 ) ;
#16067 = CARTESIAN_POINT ( 'NONE',  ( -19.62224577250664836, 2.401608896698385287, -8.935982437824780078 ) ) ;
#16068 = CARTESIAN_POINT ( 'NONE',  ( -23.41895983166000050, -8.299257554761000577, 7.436471366131000238 ) ) ;
#16069 = CARTESIAN_POINT ( 'NONE',  ( -1.999833674025762731, 11.65281303458884388, 4.383429770535894221 ) ) ;
#16070 = ORIENTED_EDGE ( 'NONE', *, *, #5954, .T. ) ;
#16071 = PLANE ( 'NONE',  #22288 ) ;
#16072 = CARTESIAN_POINT ( 'NONE',  ( 3.908839010041529338, 12.11978010317259624, -2.848422584409191494 ) ) ;
#16073 = EDGE_CURVE ( 'NONE', #18848, #9480, #2649, .T. ) ;
#16074 = CARTESIAN_POINT ( 'NONE',  ( 24.00016455292000117, -6.692834685703999753, -6.438753808737999407 ) ) ;
#16075 = EDGE_CURVE ( 'NONE', #13265, #93, #17461, .T. ) ;
#16076 = CARTESIAN_POINT ( 'NONE',  ( 11.75726969619406859, -1.905973412920116905, -8.794923108305912507 ) ) ;
#16077 = ORIENTED_EDGE ( 'NONE', *, *, #1737, .F. ) ;
#16078 = CARTESIAN_POINT ( 'NONE',  ( 0.000000000000000000, 28.30000000000000071, -4.618802153517000519 ) ) ;
#16079 = CARTESIAN_POINT ( 'NONE',  ( -6.106641414993810635, 16.02162000603732039, -1.041475911028451495 ) ) ;
#16080 = CARTESIAN_POINT ( 'NONE',  ( 17.89031392131000331, 9.735558222862998434, -0.5785200253907000212 ) ) ;
#16081 = CARTESIAN_POINT ( 'NONE',  ( 18.73721358075558996, 8.207010595434798716, 6.444024777827928929 ) ) ;
#16082 = ORIENTED_EDGE ( 'NONE', *, *, #9972, .F. ) ;
#16083 = CARTESIAN_POINT ( 'NONE',  ( -22.15362306480054855, -7.387026419981959080, 5.677192137557457663 ) ) ;
#16084 = CARTESIAN_POINT ( 'NONE',  ( -0.3631102237552999989, 28.93590169452000183, 2.430407043875000284 ) ) ;
#16085 = CARTESIAN_POINT ( 'NONE',  ( -12.30391327053333583, 6.613167033160651798, -13.46344878000693335 ) ) ;
#16086 = CARTESIAN_POINT ( 'NONE',  ( -1.534377289436119618, 13.80481766533376664, -5.932914363609297581 ) ) ;
#16087 = VERTEX_POINT ( 'NONE', #3027 ) ;
#16088 = CARTESIAN_POINT ( 'NONE',  ( 0.000000000000000000, 28.15000000000000213, 0.000000000000000000 ) ) ;
#16089 = DIRECTION ( 'NONE',  ( 0.000000000000000000, 1.000000000000000000, 0.000000000000000000 ) ) ;
#16090 = CARTESIAN_POINT ( 'NONE',  ( 16.10729166666666146, -1.189047888634119143, 9.084626563006764854 ) ) ;
#16091 = CARTESIAN_POINT ( 'NONE',  ( 0.1326132519488843198, 24.52237361985764252, -2.377626380141467433 ) ) ;
#16092 = CARTESIAN_POINT ( 'NONE',  ( 14.94969105441765933, 7.308427648130778387, 7.574777027619624903 ) ) ;
#16093 = CARTESIAN_POINT ( 'NONE',  ( -4.054781151688798602, 13.80041719377518561, 4.864580294094072777 ) ) ;
#16094 = CARTESIAN_POINT ( 'NONE',  ( -12.25000000000000178, 11.90766680615234030, -9.280428257930019242 ) ) ;
#16095 = DIRECTION ( 'NONE',  ( 1.000000000000000000, 0.000000000000000000, 0.000000000000000000 ) ) ;
#16096 = ORIENTED_EDGE ( 'NONE', *, *, #16757, .F. ) ;
#16097 = DIRECTION ( 'NONE',  ( 0.000000000000000000, 0.000000000000000000, 1.000000000000000000 ) ) ;
#16098 = AXIS2_PLACEMENT_3D ( 'NONE', #10071, #17456, #15619 ) ;
#16099 = CARTESIAN_POINT ( 'NONE',  ( 1.699999998870999951, 12.90000000000000036, 1.053565372968999991 ) ) ;
#16100 = AXIS2_PLACEMENT_3D ( 'NONE', #8482, #17684, #6409 ) ;
#16101 = VERTEX_POINT ( 'NONE', #15955 ) ;
#16102 = CARTESIAN_POINT ( 'NONE',  ( 0.6689641713224000474, 25.78843094911999856, 2.455688058221999981 ) ) ;
#16103 = CARTESIAN_POINT ( 'NONE',  ( 6.073936677003999307, 14.07872263210999364, 0.3711081957835999368 ) ) ;
#16104 = CARTESIAN_POINT ( 'NONE',  ( 11.22311500625219338, -2.002057944114464139, -12.49998975379739186 ) ) ;
#16105 = DIRECTION ( 'NONE',  ( 0.000000000000000000, 0.000000000000000000, 1.000000000000000000 ) ) ;
#16106 = CARTESIAN_POINT ( 'NONE',  ( 0.6543697108981982868, 27.76666666666666572, -2.434931691670790155 ) ) ;
#16107 = CARTESIAN_POINT ( 'NONE',  ( -4.750000000000000000, 21.89999999999999858, 0.000000000000000000 ) ) ;
#16108 = AXIS2_PLACEMENT_3D ( 'NONE', #6610, #23307, #10124 ) ;
#16109 = ORIENTED_EDGE ( 'NONE', *, *, #2740, .T. ) ;
#16110 = CARTESIAN_POINT ( 'NONE',  ( 2.184465970885649089, 30.16753006952333038, 1.259047450927240241 ) ) ;
#16111 = DIRECTION ( 'NONE',  ( 0.000000000000000000, 0.000000000000000000, 1.000000000000000000 ) ) ;
#16112 = CARTESIAN_POINT ( 'NONE',  ( 0.000000000000000000, 22.00000000000000000, 0.000000000000000000 ) ) ;
#16113 = EDGE_CURVE ( 'NONE', #15925, #21756, #12720, .T. ) ;
#16114 = ORIENTED_EDGE ( 'NONE', *, *, #6152, .T. ) ;
#16115 = CARTESIAN_POINT ( 'NONE',  ( -18.98973358726000171, -8.519062351032999914, 5.466345576189000077 ) ) ;
#16116 = CIRCLE ( 'NONE', #3748, 12.50000000000000000 ) ;
#16117 = CARTESIAN_POINT ( 'NONE',  ( 1.958365003997999843, 25.72990814437000040, -0.6262921420760999558 ) ) ;
#16118 = CARTESIAN_POINT ( 'NONE',  ( 14.88765803210585936, 10.27488610670529567, -1.076485988655981219 ) ) ;
#16119 = CARTESIAN_POINT ( 'NONE',  ( 0.000000000000000000, 23.00000000000000000, 0.000000000000000000 ) ) ;
#16120 = CARTESIAN_POINT ( 'NONE',  ( 2.009621439914000440, 30.44153028435000152, 0.8133916002304999449 ) ) ;
#16121 = CARTESIAN_POINT ( 'NONE',  ( 13.59412034164153127, 6.790033948132051300, -5.939210046344768124 ) ) ;
#16122 = CARTESIAN_POINT ( 'NONE',  ( -4.143293793513998402, 12.24260701129999163, -2.395728961457999961 ) ) ;
#16123 = EDGE_LOOP ( 'NONE', ( #8485, #6438 ) ) ;
#16124 = CARTESIAN_POINT ( 'NONE',  ( -21.61930420454665480, 5.669944305763950254, -7.377697031876467193 ) ) ;
#16125 = ORIENTED_EDGE ( 'NONE', *, *, #23855, .F. ) ;
#16126 = CARTESIAN_POINT ( 'NONE',  ( -14.25243324638999809, -7.716878364870000340, -11.63397459621999985 ) ) ;
#16127 = DIRECTION ( 'NONE',  ( 1.000000000000000000, 0.000000000000000000, 0.000000000000000000 ) ) ;
#16128 = CONICAL_SURFACE ( 'NONE', #15342, 4.309401076758999416, 1.119376321708719590 ) ;
#16129 = ORIENTED_EDGE ( 'NONE', *, *, #16310, .T. ) ;
#16130 = CARTESIAN_POINT ( 'NONE',  ( 2.500000000000000000, 30.00000000000000000, 0.000000000000000000 ) ) ;
#16131 = CARTESIAN_POINT ( 'NONE',  ( 17.05208333333332149, 2.384110632780776395, -8.871840809039129638 ) ) ;
#16132 = AXIS2_PLACEMENT_3D ( 'NONE', #315, #13043, #5781 ) ;
#16133 = CARTESIAN_POINT ( 'NONE',  ( 12.00000000000000000, -3.587209763994826162, -8.231553737011857663 ) ) ;
#16134 = CARTESIAN_POINT ( 'NONE',  ( 24.50000000000000000, 1.022558425347698252, -12.50000000000000000 ) ) ;
#16135 = AXIS2_PLACEMENT_3D ( 'NONE', #20794, #10511, #5175 ) ;
#16136 = VERTEX_POINT ( 'NONE', #17806 ) ;
#16137 = FACE_OUTER_BOUND ( 'NONE', #23858, .T. ) ;
#16138 = CARTESIAN_POINT ( 'NONE',  ( 13.49999999999999822, 7.972579677993858027, 5.894026230626296048 ) ) ;
#16139 = SURFACE_SIDE_STYLE ('',( #1385 ) ) ;
#16140 = EDGE_CURVE ( 'NONE', #22330, #23444, #23349, .T. ) ;
#16141 = EDGE_LOOP ( 'NONE', ( #2948, #3473, #12416, #15283 ) ) ;
#16142 = CARTESIAN_POINT ( 'NONE',  ( -22.85864681265000087, 6.094397095768999684, 7.552485123145999957 ) ) ;
#16143 = DIRECTION ( 'NONE',  ( -0.000000000000000000, 1.000000000000000000, 0.000000000000000000 ) ) ;
#16144 = CARTESIAN_POINT ( 'NONE',  ( 21.11742861857828402, -10.38876745042508887, -1.818149675393893272 ) ) ;
#16145 = DIRECTION ( 'NONE',  ( -1.000000000000000000, 0.000000000000000000, 0.000000000000000000 ) ) ;
#16146 = CARTESIAN_POINT ( 'NONE',  ( 16.73436614837550351, 10.39850575958874046, 0.1513134148926907341 ) ) ;
#16147 = CIRCLE ( 'NONE', #18471, 4.750000000000000000 ) ;
#16148 = STYLED_ITEM ( 'NONE', ( #6593 ), #872 ) ;
#16149 = CARTESIAN_POINT ( 'NONE',  ( -18.48849577250666343, -7.991465547029055649, 4.605847420430258410 ) ) ;
#16150 = CARTESIAN_POINT ( 'NONE',  ( -0.9467213981002000622, 29.56141545196999942, 2.143184182326999920 ) ) ;
#16151 = CARTESIAN_POINT ( 'NONE',  ( -15.96111329461999695, 9.155832847151000209, -3.339520933045000195 ) ) ;
#16152 = EDGE_CURVE ( 'NONE', #11775, #9971, #10889, .T. ) ;
#16153 = CARTESIAN_POINT ( 'NONE',  ( 1.506643486780510299, 29.90540180240715529, -1.547753345910543699 ) ) ;
#16154 = ORIENTED_EDGE ( 'NONE', *, *, #4489, .T. ) ;
#16155 = CARTESIAN_POINT ( 'NONE',  ( 23.62661714482716135, -8.104942212434002258, 4.670640012506109606 ) ) ;
#16156 = CARTESIAN_POINT ( 'NONE',  ( 20.91190086703999995, -8.572222040414001043, 7.535479936335000239 ) ) ;
#16157 = CARTESIAN_POINT ( 'NONE',  ( 23.42032133463317578, -4.048152030985803229, -9.797826222544841812 ) ) ;
#16158 = FACE_OUTER_BOUND ( 'NONE', #2041, .T. ) ;
#16159 = ORIENTED_EDGE ( 'NONE', *, *, #18437, .F. ) ;
#16160 = SHAPE_REPRESENTATION ( 'Valve Operating Stem', ( #4390 ), #23331 ) ;
#16161 = LINE ( 'NONE', #8673, #1781 ) ;
#16162 = CARTESIAN_POINT ( 'NONE',  ( 4.946118329716994388, 14.26837597718816397, -3.850108340392321526 ) ) ;
#16163 = B_SPLINE_CURVE_WITH_KNOTS ( 'NONE', 3,
 ( #13735, #10489, #8424, #2732, #15663, #21133, #15792, #1021, #13985, #21010, #11813, #21377, #1157, #4544, #17875, #11938, #6477, #19323, #4794, #12177, #10114, #8299, #2972, #15907, #10363, #21857, #9020, #16391, #9135, #10953, #12538, #12877 ),
 .UNSPECIFIED., .F., .F.,
 ( 4, 2, 2, 2, 2, 2, 2, 2, 2, 2, 2, 2, 2, 2, 2, 4 ),
 ( 0.000000000000000000, 0.1250000000000008882, 0.1875000000000012212, 0.2187500000000014988, 0.2500000000000017764, 0.3125000000000019429, 0.3437500000000021649, 0.3750000000000023870, 0.5000000000000026645, 0.5625000000000026645, 0.5937500000000025535, 0.6250000000000024425, 0.6875000000000019984, 0.7187500000000017764, 0.7500000000000015543, 1.000000000000000000 ),
 .UNSPECIFIED. ) ;
#16164 = CONICAL_SURFACE ( 'NONE', #22352, 2.849999993810000021, 0.7853981633972997312 ) ;
#16165 = CARTESIAN_POINT ( 'NONE',  ( -2.134826703869001197, 11.69852116739000358, -4.295920201858003828 ) ) ;
#16166 = ORIENTED_EDGE ( 'NONE', *, *, #2419, .F. ) ;
#16167 = CARTESIAN_POINT ( 'NONE',  ( 16.21856375731000099, 2.595497835609000159, 8.825947828509001170 ) ) ;
#16168 = VERTEX_POINT ( 'NONE', #13254 ) ;
#16169 = CARTESIAN_POINT ( 'NONE',  ( -0.2537098930414913855, 27.01480801923332820, 2.155742384934690392 ) ) ;
#16170 = APPLICATION_PROTOCOL_DEFINITION ( 'draft international standard', 'automotive_design', 1998, #8513 ) ;
#16171 = CIRCLE ( 'NONE', #1868, 10.59999999999999964 ) ;
#16172 = CARTESIAN_POINT ( 'NONE',  ( 0.000000000000000000, 28.00000000000000000, 0.000000000000000000 ) ) ;
#16173 = EDGE_CURVE ( 'NONE', #3985, #14395, #9064, .T. ) ;
#16174 = ORIENTED_EDGE ( 'NONE', *, *, #10159, .T. ) ;
#16175 = CARTESIAN_POINT ( 'NONE',  ( 0.000000000000000000, 9.100092063578999912, 0.000000000000000000 ) ) ;
#16176 = CIRCLE ( 'NONE', #18139, 10.59999999999999964 ) ;
#16177 = CARTESIAN_POINT ( 'NONE',  ( -4.103062808073617340, 15.05306268770272204, -4.547585820430672499 ) ) ;
#16178 = CARTESIAN_POINT ( 'NONE',  ( -22.67025935411000148, 10.14480762656000046, -0.3150725993096000210 ) ) ;
#16179 = CARTESIAN_POINT ( 'NONE',  ( -19.62077096955999878, 4.445609397689999298, -8.787304043923001018 ) ) ;
#16180 = CARTESIAN_POINT ( 'NONE',  ( 18.52595833333332109, -7.314397928097276846, -5.620981225341208365 ) ) ;
#16181 = CARTESIAN_POINT ( 'NONE',  ( 0.000000000000000000, 21.50000000000000000, 0.000000000000000000 ) ) ;
#16182 = CARTESIAN_POINT ( 'NONE',  ( -1.488838795626273637, 27.10843084945087256, 1.583244740691588159 ) ) ;
#16183 = AXIS2_PLACEMENT_3D ( 'NONE', #13033, #13597, #16668 ) ;
#16184 = CARTESIAN_POINT ( 'NONE',  ( 4.000000000000000000, 26.20000000000000284, -2.309401076759000304 ) ) ;
#16185 = EDGE_CURVE ( 'NONE', #12159, #20571, #5869, .T. ) ;
#16186 = CARTESIAN_POINT ( 'NONE',  ( 1.299491417509237579, 30.72164040778775274, -1.726027442315023697 ) ) ;
#16187 = ORIENTED_EDGE ( 'NONE', *, *, #5844, .T. ) ;
#16188 = CARTESIAN_POINT ( 'NONE',  ( -0.6950034797113096019, 26.37418302490043587, -4.217541707417931995 ) ) ;
#16189 = CARTESIAN_POINT ( 'NONE',  ( 3.700975972481636678, 14.35177231820836319, 4.880830331095896035 ) ) ;
#16190 = CARTESIAN_POINT ( 'NONE',  ( -1.675531247043999805, 27.15413313894999803, 1.812579491195999815 ) ) ;
#16191 = AXIS2_PLACEMENT_3D ( 'NONE', #16226, #12717, #10904 ) ;
#16192 = CARTESIAN_POINT ( 'NONE',  ( -4.750000000000000000, 20.10000000000000142, 0.000000000000000000 ) ) ;
#16193 = CARTESIAN_POINT ( 'NONE',  ( -1.197800277839999872, 28.25864211381999880, -1.954613887214999846 ) ) ;
#16194 = VECTOR ( 'NONE', #13646, 1000.000000000000000 ) ;
#16195 = VECTOR ( 'NONE', #3828, 1000.000000000000000 ) ;
#16196 = CARTESIAN_POINT ( 'NONE',  ( -3.558068219325319692, 12.01240764178410281, 3.274221823266413534 ) ) ;
#16197 = ORIENTED_EDGE ( 'NONE', *, *, #23223, .T. ) ;
#16198 = CARTESIAN_POINT ( 'NONE',  ( -6.042815982636000172, 21.50000000000000000, -1.000000000000000000 ) ) ;
#16199 = DIRECTION ( 'NONE',  ( 0.000000000000000000, 0.000000000000000000, 1.000000000000000000 ) ) ;
#16200 = AXIS2_PLACEMENT_3D ( 'NONE', #23410, #10355, #17866 ) ;
#16201 = CARTESIAN_POINT ( 'NONE',  ( -21.05832910583999862, 9.211679941677999750, 0.000000000000000000 ) ) ;
#16202 = CARTESIAN_POINT ( 'NONE',  ( -21.31697087121332856, 9.218317199134103745, 1.206801847291242513 ) ) ;
#16203 = ORIENTED_EDGE ( 'NONE', *, *, #5417, .F. ) ;
#16204 = ADVANCED_FACE ( 'NONE', ( #20097 ), #1571, .F. ) ;
#16205 = EDGE_CURVE ( 'NONE', #21708, #17401, #368, .T. ) ;
#16206 = CARTESIAN_POINT ( 'NONE',  ( -5.529771451991000397, -1.199084044040999915E-14, 0.000000000000000000 ) ) ;
#16207 = FACE_OUTER_BOUND ( 'NONE', #14649, .T. ) ;
#16208 = CARTESIAN_POINT ( 'NONE',  ( 13.17375142130999954, -7.436937191241000278, 6.115943375764999246 ) ) ;
#16209 = CARTESIAN_POINT ( 'NONE',  ( 18.72046758034523961, 8.553234081428245261, 5.969153472710740260 ) ) ;
#16210 = CIRCLE ( 'NONE', #2271, 1.600000000000000089 ) ;
#16211 = ORIENTED_EDGE ( 'NONE', *, *, #3199, .F. ) ;
#16212 = LINE ( 'NONE', #15718, #8095 ) ;
#16213 = CARTESIAN_POINT ( 'NONE',  ( -0.9741922325766999569, 29.81343306396000159, 2.543667732614000254 ) ) ;
#16214 = CARTESIAN_POINT ( 'NONE',  ( -24.50000000000000000, 10.82531754731000007, -6.250000000000000000 ) ) ;
#16215 = DIRECTION ( 'NONE',  ( 0.8500000008401347174, 0.000000000000000000, 0.5267826862870217397 ) ) ;
#16216 = CIRCLE ( 'NONE', #20106, 4.000000000000000000 ) ;
#16217 = B_SPLINE_CURVE_WITH_KNOTS ( 'NONE', 3,
 ( #23895, #7302, #7539, #14802, #22197, #1980, #14693, #22085, #12874, #3678, #20274, #11069 ),
 .UNSPECIFIED., .F., .F.,
 ( 4, 1, 1, 1, 1, 2, 2, 4 ),
 ( 0.000000000000000000, 0.2499999999999986122, 0.3749999999999980571, 0.4374999999999979461, 0.4687499999999978351, 0.4843749999999980016, 0.4999999999999981126, 1.000000000000000000 ),
 .UNSPECIFIED. ) ;
#16218 = EDGE_LOOP ( 'NONE', ( #4412, #18166, #7113, #68, #18494, #10436 ) ) ;
#16219 = AXIS2_PLACEMENT_3D ( 'NONE', #8633, #20014, #15996 ) ;
#16220 = CARTESIAN_POINT ( 'NONE',  ( 0.000000000000000000, 15.09999999999999964, 0.000000000000000000 ) ) ;
#16221 = LINE ( 'NONE', #7020, #11975 ) ;
#16222 = CARTESIAN_POINT ( 'NONE',  ( 16.44741666666666546, -8.856630573480710922, 2.380283675663321663 ) ) ;
#16223 = ADVANCED_FACE ( 'NONE', ( #7808 ), #2258, .F. ) ;
#16224 = CARTESIAN_POINT ( 'NONE',  ( 2.424643331163519964E-11, 24.52694564545263844, -2.373054354547839306 ) ) ;
#16225 = EDGE_CURVE ( 'NONE', #12189, #5466, #6126, .T. ) ;
#16226 = CARTESIAN_POINT ( 'NONE',  ( -24.50000000000000000, 1.524685264937999788E-14, 0.000000000000000000 ) ) ;
#16227 = CARTESIAN_POINT ( 'NONE',  ( 2.063594504837999888E-14, 28.80370090847999975, 2.160000000000000142 ) ) ;
#16228 = AXIS2_PLACEMENT_3D ( 'NONE', #11559, #16871, #17119 ) ;
#16229 = DIRECTION ( 'NONE',  ( -0.000000000000000000, 1.000000000000000000, 0.000000000000000000 ) ) ;
#16230 = ORIENTED_EDGE ( 'NONE', *, *, #3708, .F. ) ;
#16231 = CARTESIAN_POINT ( 'NONE',  ( -11.04281598264000053, 16.43285860070444215, 0.1718092760798936858 ) ) ;
#16232 = CARTESIAN_POINT ( 'NONE',  ( 1.727343568716567690, 12.96873773180061207, 1.061322550613886140 ) ) ;
#16233 = B_SPLINE_CURVE_WITH_KNOTS ( 'NONE', 3,
 ( #10192, #4626, #8256, #851, #8503, #22891, #17458, #15980, #15621, #1104, #21211, #15866, #12383, #10315, #21086, #6307, #1227, #12015, #4496, #23130, #17582, #2930, #14186, #17832, #8618, #3056, #19397, #8377, #23256, #13940, #21583, #19769, #10444, #14062, #21334, #9943, #23010, #15744, #4749, #13690, #11887, #12134, #19271, #19522, #17706, #21455, #2685, #6428, #4870, #13812, #1595, #18299, #21928, #20123, #1819, #5228, #8868, #10560, #10679 ),
 .UNSPECIFIED., .F., .F.,
 ( 4, 2, 2, 1, 1, 1, 1, 1, 2, 2, 2, 2, 2, 1, 1, 1, 2, 2, 2, 2, 2, 2, 1, 1, 2, 2, 2, 2, 1, 1, 1, 1, 1, 2, 2, 2, 4 ),
 ( 0.000000000000000000, 0.1250000000000092704, 0.1875000000000140721, 0.2187500000000165701, 0.2343750000000176248, 0.2421875000000181799, 0.2460937500000183187, 0.2480468750000185407, 0.2490234375000186240, 0.2500000000000187628, 0.3750000000000224265, 0.4375000000000242029, 0.4687500000000250910, 0.4843750000000255351, 0.4921875000000258127, 0.4960937500000259237, 0.4980468750000259237, 0.5000000000000259792, 0.5625000000000269784, 0.6250000000000278666, 0.6875000000000289768, 0.7187500000000294209, 0.7343750000000297540, 0.7421875000000298650, 0.7460937500000298650, 0.7500000000000299760, 0.8125000000000306422, 0.8437500000000309752, 0.8593750000000310862, 0.8671875000000311973, 0.8710937500000313083, 0.8730468750000311973, 0.8740234375000311973, 0.8745117187500313083, 0.8750000000000314193, 0.9375000000000157652, 1.000000000000000000 ),
 .UNSPECIFIED. ) ;
#16234 = ORIENTED_EDGE ( 'NONE', *, *, #14565, .T. ) ;
#16235 = CIRCLE ( 'NONE', #2703, 1.750000000000000000 ) ;
#16236 = CARTESIAN_POINT ( 'NONE',  ( 1.775541456815999952, 24.57013026871000250, -2.083124542231000298 ) ) ;
#16237 = CARTESIAN_POINT ( 'NONE',  ( 5.259117788274003225, 14.75723778743001802, 3.160412202088998423 ) ) ;
#16238 = CARTESIAN_POINT ( 'NONE',  ( 11.06619116163201078, 0.4983756421073917697, -12.49999828234741805 ) ) ;
#16239 = CARTESIAN_POINT ( 'NONE',  ( 19.32833333333333670, 8.869419113210506467, 2.676869261568202596 ) ) ;
#16240 = LINE ( 'NONE', #7037, #13297 ) ;
#16241 = CARTESIAN_POINT ( 'NONE',  ( -1.315747796919693791, 23.71666666666667211, -1.829618100335548725 ) ) ;
#16242 = EDGE_LOOP ( 'NONE', ( #11714, #19765, #11251, #4879, #3053 ) ) ;
#16243 = CARTESIAN_POINT ( 'NONE',  ( -18.43943555148999991, -2.412201287215999912, -10.06532802039999908 ) ) ;
#16244 = CIRCLE ( 'NONE', #20128, 11.50000000000000000 ) ;
#16245 = CARTESIAN_POINT ( 'NONE',  ( -1.412199477822031035, 26.21336570662361964, 1.592595083443383963 ) ) ;
#16246 = CARTESIAN_POINT ( 'NONE',  ( 1.709999999999999964, 0.000000000000000000, 0.000000000000000000 ) ) ;
#16247 = ORIENTED_EDGE ( 'NONE', *, *, #18378, .T. ) ;
#16248 = CARTESIAN_POINT ( 'NONE',  ( -19.57635548768000078, 1.980828427502000055, 10.47560186498999890 ) ) ;
#16249 = DIRECTION ( 'NONE',  ( 1.000000000000000000, 0.000000000000000000, 0.000000000000000000 ) ) ;
#16250 = CARTESIAN_POINT ( 'NONE',  ( 14.54019110570222750, 2.698302716369401999, -9.963003989504706226 ) ) ;
#16251 = CARTESIAN_POINT ( 'NONE',  ( -2.000000000000000000, 28.00000000000000000, 3.464101615137999968 ) ) ;
#16252 = CARTESIAN_POINT ( 'NONE',  ( 20.41802811994999800, 7.805777114999000510, 8.035878495494999996 ) ) ;
#16253 = CARTESIAN_POINT ( 'NONE',  ( 24.24531177150999994, 0.000000000000000000, 0.000000000000000000 ) ) ;
#16254 = CARTESIAN_POINT ( 'NONE',  ( 13.57120437455812656, 6.313184194241564740, -6.461219362146199963 ) ) ;
#16255 = CARTESIAN_POINT ( 'NONE',  ( -3.536243307738002439, 12.19150164470999442, -3.169402752236001763 ) ) ;
#16256 = VERTEX_POINT ( 'NONE', #15180 ) ;
#16257 = CARTESIAN_POINT ( 'NONE',  ( -0.8020744510286262896, 26.50000000000000355, 2.262007200476410684 ) ) ;
#16258 = ORIENTED_EDGE ( 'NONE', *, *, #12823, .T. ) ;
#16259 = CARTESIAN_POINT ( 'NONE',  ( -6.043485951305999748, 16.34784564573999788, 1.000000003648999991 ) ) ;
#16260 = DIRECTION ( 'NONE',  ( 1.511005137241999593E-08, -0.9999999999999997780, 8.997177532459998026E-09 ) ) ;
#16261 = ORIENTED_EDGE ( 'NONE', *, *, #14230, .T. ) ;
#16262 = DIRECTION ( 'NONE',  ( 0.000000000000000000, 1.000000000000000000, 0.000000000000000000 ) ) ;
#16263 = CARTESIAN_POINT ( 'NONE',  ( 11.72559253310116389, -12.88358093001479432, -2.684900464184909907 ) ) ;
#16264 = CARTESIAN_POINT ( 'NONE',  ( -6.000000000000000000, 26.50000000000000000, -6.000000000000000000 ) ) ;
#16265 = CARTESIAN_POINT ( 'NONE',  ( 18.80965323898000108, 0.6517886434522999206, 11.11406264393000143 ) ) ;
#16266 = ORIENTED_EDGE ( 'NONE', *, *, #1684, .F. ) ;
#16267 = CARTESIAN_POINT ( 'NONE',  ( -11.72719613877000100, 5.763420833702999957, 14.08487056595000020 ) ) ;
#16268 = CARTESIAN_POINT ( 'NONE',  ( 13.50000000000000000, 9.165557434110747081, -2.271160277613796907 ) ) ;
#16269 = CARTESIAN_POINT ( 'NONE',  ( -6.000000000000000000, 24.99999999999999645, -115.0195023120000002 ) ) ;
#16270 = ORIENTED_EDGE ( 'NONE', *, *, #20638, .T. ) ;
#16271 = CARTESIAN_POINT ( 'NONE',  ( 20.73503899750121704, -4.285134948126297694, 9.623718970242478576 ) ) ;
#16272 = CARTESIAN_POINT ( 'NONE',  ( -2.000000000000000000, 26.50000000000000355, 3.464101615137999968 ) ) ;
#16273 = CARTESIAN_POINT ( 'NONE',  ( 15.93025666723834100, -9.681699128342794225, -3.681818963616494855 ) ) ;
#16274 = CARTESIAN_POINT ( 'NONE',  ( -19.28992806661999992, -9.239313293073999844, 5.311636531851000598 ) ) ;
#16275 = CARTESIAN_POINT ( 'NONE',  ( -2.186232643004999865, 30.22719044073999939, -0.09498792041393000485 ) ) ;
#16276 = CONICAL_SURFACE ( 'NONE', #5833, 4.309401076758999416, 1.119376321708719590 ) ;
#16277 = CARTESIAN_POINT ( 'NONE',  ( -12.30476703115999904, 8.600742661000001732, -2.211712587549000020 ) ) ;
#16278 = CARTESIAN_POINT ( 'NONE',  ( 0.8953157965490899928, 29.94952453685389315, -1.965511115583160384 ) ) ;
#16279 = VERTEX_POINT ( 'NONE', #1674 ) ;
#16280 = CARTESIAN_POINT ( 'NONE',  ( -24.16119556692343551, -4.108075932065574420, 12.49973851152546089 ) ) ;
#16281 = CARTESIAN_POINT ( 'NONE',  ( 11.92450592357671368, 13.18099206878371632, -2.169941377000860872 ) ) ;
#16282 = CARTESIAN_POINT ( 'NONE',  ( 22.34213275544827937, 8.806011279328485486, 5.853390237427837484 ) ) ;
#16283 = CARTESIAN_POINT ( 'NONE',  ( -0.9598074410945768298, 23.62549911315723605, -1.896475888262205478 ) ) ;
#16284 = ORIENTED_EDGE ( 'NONE', *, *, #10409, .F. ) ;
#16285 = EDGE_CURVE ( 'NONE', #4621, #18634, #1558, .T. ) ;
#16286 = CARTESIAN_POINT ( 'NONE',  ( 24.18393254356834632, -8.381833107684220963, -10.48223919692640393 ) ) ;
#16287 = DIRECTION ( 'NONE',  ( 0.000000000000000000, 0.000000000000000000, 1.000000000000000000 ) ) ;
#16288 = CARTESIAN_POINT ( 'NONE',  ( 3.823771652646001051, 12.06071475417000194, -3.000030641231999695 ) ) ;
#16289 = ORIENTED_EDGE ( 'NONE', *, *, #14699, .T. ) ;
#16290 = CARTESIAN_POINT ( 'NONE',  ( 0.000000000000000000, -9.000000000000000000, 0.000000000000000000 ) ) ;
#16291 = VERTEX_POINT ( 'NONE', #10775 ) ;
#16292 = CARTESIAN_POINT ( 'NONE',  ( 1.330759560658445029, 26.31212306573571524, 1.751177748763361075 ) ) ;
#16293 = ITEM_DEFINED_TRANSFORMATION ( 'NONE', 'NONE', #13268,  #4390 ) ;
#16294 = CARTESIAN_POINT ( 'NONE',  ( -14.49454818139149737, -1.035381146742340386, -12.50000698752768180 ) ) ;
#16295 = B_SPLINE_CURVE_WITH_KNOTS ( 'NONE', 3,
 ( #9335, #14773, #9453, #16707, #118, #1830, #16827, #5580, #7154, #18204, #231, #1605, #9217, #23864, #22406, #1711, #20358, #5815, #7, #3429, #22169, #3766, #7506, #18309, #10813, #8990, #7390, #16361, #23750, #21938, #20132, #14889 ),
 .UNSPECIFIED., .F., .F.,
 ( 4, 2, 2, 2, 2, 2, 2, 2, 1, 2, 2, 2, 1, 1, 1, 2, 2, 4 ),
 ( 0.000000000000000000, 0.2500000000000005551, 0.3750000000000008327, 0.4374999999999986122, 0.4687499999999996114, 0.5000000000000005551, 0.6250000000000122125, 0.6875000000000178746, 0.7187500000000202061, 0.7343750000000223155, 0.7500000000000243139, 0.8125000000000297540, 0.8437500000000324185, 0.8593750000000328626, 0.8671875000000330846, 0.8710937500000331957, 0.8750000000000334177, 1.000000000000000000 ),
 .UNSPECIFIED. ) ;
#16296 = EDGE_CURVE ( 'NONE', #6372, #2681, #12817, .T. ) ;
#16297 = ORIENTED_EDGE ( 'NONE', *, *, #6838, .F. ) ;
#16298 = CARTESIAN_POINT ( 'NONE',  ( -15.04355420454667325, -9.057328963212048833, 1.185474641176787802 ) ) ;
#16299 = CARTESIAN_POINT ( 'NONE',  ( -22.02791261424000169, -5.912491595945999379, 8.228415427290999062 ) ) ;
#16300 = CARTESIAN_POINT ( 'NONE',  ( -13.66394044103999938, 9.112107522246999380, -2.343211941154000222 ) ) ;
#16301 = CARTESIAN_POINT ( 'NONE',  ( -6.143111768200996359, 14.96860033859000971, -3.824985432946004682 ) ) ;
#16302 = CARTESIAN_POINT ( 'NONE',  ( -22.02842343893881250, 9.533828963910684351, 5.524295927557433927 ) ) ;
#16303 = CARTESIAN_POINT ( 'NONE',  ( -1.781275706426519445, 27.08192969757271484, 1.242185054261912391 ) ) ;
#16304 = DIRECTION ( 'NONE',  ( -0.7071067811905932254, -0.7071067811824932603, -1.099460899159990341E-07 ) ) ;
#16305 = CARTESIAN_POINT ( 'NONE',  ( 0.000000000000000000, 29.69999999999999929, 4.618802153517000519 ) ) ;
#16306 = ORIENTED_EDGE ( 'NONE', *, *, #22837, .F. ) ;
#16307 = CARTESIAN_POINT ( 'NONE',  ( 24.00016455292000117, -9.066063387507998783, 2.014468017461000127 ) ) ;
#16308 = DIRECTION ( 'NONE',  ( 0.000000000000000000, 1.000000000000000000, 0.000000000000000000 ) ) ;
#16309 = CARTESIAN_POINT ( 'NONE',  ( 1.831974274068000064, 25.68369850838000090, 0.9334375154566999511 ) ) ;
#16310 = EDGE_CURVE ( 'NONE', #15754, #23789, #4985, .T. ) ;
#16311 = AXIS2_PLACEMENT_3D ( 'NONE', #13939, #4748, #10191 ) ;
#16312 = CARTESIAN_POINT ( 'NONE',  ( 2.089231778180999921, 25.80521896305999974, 0.4700916780637000580 ) ) ;
#16313 = CARTESIAN_POINT ( 'NONE',  ( 4.467732293902829888, 12.30836910800113060, 1.873439991674330285 ) ) ;
#16314 = ORIENTED_EDGE ( 'NONE', *, *, #10313, .T. ) ;
#16315 = CARTESIAN_POINT ( 'NONE',  ( -23.75856372112291481, -13.93375672973999890, 0.09623563749425553815 ) ) ;
#16316 = CARTESIAN_POINT ( 'NONE',  ( 4.431702799432089002, 12.29558746875803976, -1.954764367055115803 ) ) ;
#16317 = CARTESIAN_POINT ( 'NONE',  ( -17.72676253787999912, 9.126185377371999863, 0.000000000000000000 ) ) ;
#16318 = VECTOR ( 'NONE', #2658, 1000.000000000000000 ) ;
#16319 = CARTESIAN_POINT ( 'NONE',  ( -21.05242920454665878, 4.638983325918172085, 8.048956833715248393 ) ) ;
#16320 = ORIENTED_EDGE ( 'NONE', *, *, #14119, .F. ) ;
#16321 = EDGE_CURVE ( 'NONE', #23625, #17141, #23535, .T. ) ;
#16322 = CARTESIAN_POINT ( 'NONE',  ( -1.259047450927199163, 24.13333333333333641, 2.184465970885673070 ) ) ;
#16323 = CARTESIAN_POINT ( 'NONE',  ( -16.10172087121332396, 7.264650085109141564, -5.582749836826320866 ) ) ;
#16324 = CARTESIAN_POINT ( 'NONE',  ( 16.02562642131000104, 9.437180554902999674, -2.258696805882000280 ) ) ;
#16325 = CARTESIAN_POINT ( 'NONE',  ( 18.80165828517651150, 6.582155627870158732, 8.096495908088112259 ) ) ;
#16326 = CARTESIAN_POINT ( 'NONE',  ( 4.000000000000000000, 28.00000000000000000, 0.000000000000000000 ) ) ;
#16327 = CARTESIAN_POINT ( 'NONE',  ( -2.135391386772000022, 30.15892637698999934, 0.2566162452548999551 ) ) ;
#16328 = B_SPLINE_CURVE_WITH_KNOTS ( 'NONE', 3,
 ( #9648, #4315, #17270, #670, #18005, #23197, #23435, #2865 ),
 .UNSPECIFIED., .F., .F.,
 ( 4, 2, 2, 4 ),
 ( 0.000000000000000000, 0.2499999999999998890, 0.4999999999999997780, 1.000000000000000000 ),
 .UNSPECIFIED. ) ;
#16329 = DIRECTION ( 'NONE',  ( 0.000000000000000000, 1.000000000000000000, 0.000000000000000000 ) ) ;
#16330 = CARTESIAN_POINT ( 'NONE',  ( 13.49999999999999822, -9.119346161239230142, 3.853256094986214908 ) ) ;
#16331 = CIRCLE ( 'NONE', #20986, 3.100000000000000089 ) ;
#16332 = ORIENTED_EDGE ( 'NONE', *, *, #10757, .T. ) ;
#16333 = ADVANCED_FACE ( 'NONE', ( #16207 ), #14641, .T. ) ;
#16334 = DIRECTION ( 'NONE',  ( 0.000000000000000000, -1.000000000000000000, 0.000000000000000000 ) ) ;
#16335 = CARTESIAN_POINT ( 'NONE',  ( 23.31148506108999996, -6.143795288837999635, -9.535093121894000490 ) ) ;
#16336 = DIRECTION ( 'NONE',  ( -0.000000000000000000, 1.000000000000000000, -0.000000000000000000 ) ) ;
#16337 = CARTESIAN_POINT ( 'NONE',  ( 24.50000000000000000, -2.116736914405999759, 10.36413001332999961 ) ) ;
#16338 = CARTESIAN_POINT ( 'NONE',  ( -4.085530525064275054, 13.77267084576624079, 4.872318283361749991 ) ) ;
#16339 = CARTESIAN_POINT ( 'NONE',  ( -4.943683218093997134, 12.51395247683998058, -0.06195390666880997571 ) ) ;
#16340 = ADVANCED_FACE ( 'NONE', ( #23713 ), #5370, .T. ) ;
#16341 = CARTESIAN_POINT ( 'NONE',  ( 12.50000000000000000, 13.93375672974000068, 0.000000000000000000 ) ) ;
#16342 = VERTEX_POINT ( 'NONE', #2353 ) ;
#16343 = CARTESIAN_POINT ( 'NONE',  ( 1.350509132759432740, 30.61094555582495502, 2.026494689485950573 ) ) ;
#16344 = ADVANCED_FACE ( 'NONE', ( #4668 ), #12052, .T. ) ;
#16345 = B_SPLINE_CURVE_WITH_KNOTS ( 'NONE', 3,
 ( #8571, #2091, #3796, #20739 ),
 .UNSPECIFIED., .F., .F.,
 ( 4, 4 ),
 ( 0.000000000000000000, 1.000000000000000000 ),
 .UNSPECIFIED. ) ;
#16346 = CARTESIAN_POINT ( 'NONE',  ( -10.90000000000000036, 1.358133300253999998E-14, 0.000000000000000000 ) ) ;
#16347 = ORIENTED_EDGE ( 'NONE', *, *, #4552, .F. ) ;
#16348 = CARTESIAN_POINT ( 'NONE',  ( -2.152918217223999786, 24.53250749508999817, -0.1897174181730999776 ) ) ;
#16349 = CARTESIAN_POINT ( 'NONE',  ( 6.132698908501003743, 14.49462454531001754, 0.1095711543429000179 ) ) ;
#16350 = CARTESIAN_POINT ( 'NONE',  ( 12.28022044528181311, -5.662962823250645705, -12.50000000000071942 ) ) ;
#16351 = AXIS2_PLACEMENT_3D ( 'NONE', #10449, #23377, #18069 ) ;
#16352 = CARTESIAN_POINT ( 'NONE',  ( 19.66566666666665952, 1.030022276571363804, 9.215888979280039806 ) ) ;
#16353 = CARTESIAN_POINT ( 'NONE',  ( -5.539688061797002128, 16.26872474856999773, -2.643098357780001351 ) ) ;
#16354 = CARTESIAN_POINT ( 'NONE',  ( -2.443333333333321811, 23.94333333333336356, -0.4702601233135134673 ) ) ;
#16355 = EDGE_CURVE ( 'NONE', #10321, #2748, #10527, .T. ) ;
#16356 = ORIENTED_EDGE ( 'NONE', *, *, #10862, .T. ) ;
#16357 = CARTESIAN_POINT ( 'NONE',  ( -18.60180781823000018, -9.793299576559000741, 0.7034231180304000297 ) ) ;
#16358 = CARTESIAN_POINT ( 'NONE',  ( -0.02719911563634819923, 26.24132134161193264, 2.156122861279925917 ) ) ;
#16359 = CARTESIAN_POINT ( 'NONE',  ( 11.00000000000000000, 0.000000000000000000, 0.000000000000000000 ) ) ;
#16360 = VERTEX_POINT ( 'NONE', #15540 ) ;
#16361 = CARTESIAN_POINT ( 'NONE',  ( -10.83632914535144920, 15.36350589476169937, -1.682004463026524066 ) ) ;
#16362 = CARTESIAN_POINT ( 'NONE',  ( 2.101206698852999821, 24.06483916994999817, 0.4292744954273000624 ) ) ;
#16363 = CARTESIAN_POINT ( 'NONE',  ( 14.80091196040006984, 9.530334370396518651, -3.997581378746529968 ) ) ;
#16364 = CARTESIAN_POINT ( 'NONE',  ( -4.000000000000000000, 24.50000000000000000, 2.309401076759000304 ) ) ;
#16365 = CARTESIAN_POINT ( 'NONE',  ( 23.35477952741999985, -0.2659429092311000331, -11.28040236504000049 ) ) ;
#16366 = LINE ( 'NONE', #12745, #18873 ) ;
#16367 = CARTESIAN_POINT ( 'NONE',  ( 13.80060059804144501, 9.025283489161427752, -0.03376589920026255159 ) ) ;
#16368 = CARTESIAN_POINT ( 'NONE',  ( -4.660137320655001858, 12.58447456225998984, -1.233398502364998484 ) ) ;
#16369 = CARTESIAN_POINT ( 'NONE',  ( -22.26176253788000281, -9.242562415387000740, 0.000000000000000000 ) ) ;
#16370 = EDGE_CURVE ( 'NONE', #16646, #17341, #8466, .T. ) ;
#16371 = ORIENTED_EDGE ( 'NONE', *, *, #4832, .T. ) ;
#16372 = DIRECTION ( 'NONE',  ( 1.000000000000000000, 0.000000000000000000, 0.000000000000000000 ) ) ;
#16373 = CARTESIAN_POINT ( 'NONE',  ( -11.00000000000000000, 1.359357947053999856E-14, 0.000000000000000000 ) ) ;
#16374 = ORIENTED_EDGE ( 'NONE', *, *, #21183, .F. ) ;
#16375 = CARTESIAN_POINT ( 'NONE',  ( 2.062405688592416908, 30.08447145040267401, -1.608325556874773410 ) ) ;
#16376 = CARTESIAN_POINT ( 'NONE',  ( 17.12766666666665571, 4.588260261546838414, -7.960951565941960517 ) ) ;
#16377 = CARTESIAN_POINT ( 'NONE',  ( 24.50000000000000000, 0.000000000000000000, 0.000000000000000000 ) ) ;
#16378 = CARTESIAN_POINT ( 'NONE',  ( 16.46379156698999680, 10.47191086351999978, -3.587674625133999928 ) ) ;
#16379 = EDGE_CURVE ( 'NONE', #11959, #9355, #9984, .T. ) ;
#16380 = VERTEX_POINT ( 'NONE', #23047 ) ;
#16381 = CARTESIAN_POINT ( 'NONE',  ( -10.10541006585000012, 9.582871899720000641, 11.36777908496999956 ) ) ;
#16382 = CARTESIAN_POINT ( 'NONE',  ( 13.50000000000000000, 8.796014925232748638, 4.387719908057123419 ) ) ;
#16383 = CARTESIAN_POINT ( 'NONE',  ( 2.000000000000000000, 28.00000000000000000, -3.464101615137999968 ) ) ;
#16384 = ORIENTED_EDGE ( 'NONE', *, *, #11500, .T. ) ;
#16385 = CARTESIAN_POINT ( 'NONE',  ( 20.49972230760754854, 4.054746914731249596, 9.712109459497844099 ) ) ;
#16386 = CARTESIAN_POINT ( 'NONE',  ( -24.50000000000000000, -10.30000000000000071, 0.000000000000000000 ) ) ;
#16387 = CARTESIAN_POINT ( 'NONE',  ( 16.06122657628786143, -7.038767995605364369, -7.618814742105207038 ) ) ;
#16388 = DIRECTION ( 'NONE',  ( 0.000000000000000000, 1.000000000000000000, 0.000000000000000000 ) ) ;
#16389 = AXIS2_PLACEMENT_3D ( 'NONE', #19944, #15812, #1175 ) ;
#16390 = B_SPLINE_CURVE_WITH_KNOTS ( 'NONE', 3,
 ( #707, #17308, #17808, #2785, #17556, #830, #8476, #22987, #12234, #10171, #952, #1204, #22869, #15600, #15716, #8233, #15483, #8595 ),
 .UNSPECIFIED., .F., .F.,
 ( 4, 2, 2, 2, 2, 2, 2, 2, 4 ),
 ( 0.000000000000000000, 0.1250000000000000000, 0.2500000000000000000, 0.3750000000000000000, 0.5000000000000000000, 0.6250000000000000000, 0.7500000000000000000, 0.8750000000000000000, 1.000000000000000000 ),
 .UNSPECIFIED. ) ;
#16391 = CARTESIAN_POINT ( 'NONE',  ( -14.44600769525627904, -12.24671445775785728, 3.788037462221160112 ) ) ;
#16392 = CARTESIAN_POINT ( 'NONE',  ( -4.000000000000115463, 27.99999999999976552, -0.1904558375376560198 ) ) ;
#16393 = CARTESIAN_POINT ( 'NONE',  ( 1.724429579411198787, 29.88617415415703604, -1.300538479143458215 ) ) ;
#16394 = ORIENTED_EDGE ( 'NONE', *, *, #12889, .F. ) ;
#16395 = CARTESIAN_POINT ( 'NONE',  ( 20.35599589905567086, 10.52498947291094744, -0.1069429831477965442 ) ) ;
#16396 = CARTESIAN_POINT ( 'NONE',  ( -1.958067310766663738, 26.26028141853885245, 0.9125917284305815613 ) ) ;
#16397 = CONICAL_SURFACE ( 'NONE', #15613, 4.699999872533999756, 0.7853981633972997312 ) ;
#16398 = ORIENTED_EDGE ( 'NONE', *, *, #23265, .F. ) ;
#16399 = CARTESIAN_POINT ( 'NONE',  ( 20.43528936713000377, -9.195691514035999603, 0.000000000000000000 ) ) ;
#16400 = CARTESIAN_POINT ( 'NONE',  ( 4.835835251289409165, 14.67308180627193082, -3.769935304963333511 ) ) ;
#16401 = CARTESIAN_POINT ( 'NONE',  ( -4.910842247424000107, 12.43786476712998912, -0.3318925675130997011 ) ) ;
#16402 = ORIENTED_EDGE ( 'NONE', *, *, #21535, .F. ) ;
#16403 = CARTESIAN_POINT ( 'NONE',  ( -15.00576253787999903, -9.056359154562001024, 0.000000000000000000 ) ) ;
#16404 = CIRCLE ( 'NONE', #11003, 2.500000000000001776 ) ;
#16405 = VERTEX_POINT ( 'NONE', #6469 ) ;
#16406 = CARTESIAN_POINT ( 'NONE',  ( -3.644446339697000159, 14.33206891720999998, 4.922772686299000000 ) ) ;
#16407 = APPLICATION_PROTOCOL_DEFINITION ( 'draft international standard', 'automotive_design', 1998, #6007 ) ;
#16408 = LINE ( 'NONE', #5516, #19881 ) ;
#16409 = ORIENTED_EDGE ( 'NONE', *, *, #7395, .F. ) ;
#16410 = CARTESIAN_POINT ( 'NONE',  ( 22.24928936712999672, -9.242242329243000043, 0.000000000000000000 ) ) ;
#16411 = AXIS2_PLACEMENT_3D ( 'NONE', #3224, #10606, #16388 ) ;
#16412 = CARTESIAN_POINT ( 'NONE',  ( -20.74321913448999766, 9.448588360516998463, 3.561785475570999893 ) ) ;
#16413 = ORIENTED_CLOSED_SHELL ( 'NONE', *, #13106, .F. );
#16414 = CARTESIAN_POINT ( 'NONE',  ( -16.77694609798000158, -7.614211477670999706, 6.119569497340999753 ) ) ;
#16415 = CARTESIAN_POINT ( 'NONE',  ( -4.770933648794001058, 13.03075770454000448, -5.112134952572002788 ) ) ;
#16416 = CARTESIAN_POINT ( 'NONE',  ( -23.44385535506140172, -3.478864065003184791, 9.993471346658315824 ) ) ;
#16417 = CARTESIAN_POINT ( 'NONE',  ( -1.762470634073454390, 26.28689514065213473, 1.324303524335109783 ) ) ;
#16418 = AXIS2_PLACEMENT_3D ( 'NONE', #10581, #14781, #7162 ) ;
#16419 = CARTESIAN_POINT ( 'NONE',  ( -6.579472545193000954, 15.16114063110001986, 2.985323136169000691 ) ) ;
#16420 = FACE_OUTER_BOUND ( 'NONE', #17443, .T. ) ;
#16421 = EDGE_LOOP ( 'NONE', ( #21482, #12166, #10880, #7118 ) ) ;
#16422 = CARTESIAN_POINT ( 'NONE',  ( 23.40350286971751004, 6.148604348410775522, 7.026089829741110293 ) ) ;
#16423 = CARTESIAN_POINT ( 'NONE',  ( 2.267779804951839839, 26.36777980495183726, 5.387954023152814032E-08 ) ) ;
#16424 = CARTESIAN_POINT ( 'NONE',  ( 14.83790034821742587, -7.812907433739113117, 4.674760609328123095 ) ) ;
#16425 = CARTESIAN_POINT ( 'NONE',  ( 5.826617149234366799, 14.45297212092532213, -1.888469283984045566 ) ) ;
#16426 = CARTESIAN_POINT ( 'NONE',  ( 1.516486965307999979, 26.72937716036000211, -1.923654546119000219 ) ) ;
#16427 = CIRCLE ( 'NONE', #18009, 2.673746900119611247 ) ;
#16428 = CARTESIAN_POINT ( 'NONE',  ( 2.218588997953582442, 11.69175043203580877, 4.278498257537161287 ) ) ;
#16429 = ORIENTED_EDGE ( 'NONE', *, *, #4818, .T. ) ;
#16430 = CARTESIAN_POINT ( 'NONE',  ( -2.776765130543696447, 11.80852668188584964, -3.944772877159900215 ) ) ;
#16431 = CARTESIAN_POINT ( 'NONE',  ( -10.19258028079843825, 15.86589456477620708, 1.102853906025392350 ) ) ;
#16432 = CARTESIAN_POINT ( 'NONE',  ( -1.944928363488455325, 29.16054931928814398, -1.185957275569452296 ) ) ;
#16433 = ORIENTED_EDGE ( 'NONE', *, *, #17675, .F. ) ;
#16434 = DIRECTION ( 'NONE',  ( 0.000000000000000000, 0.000000000000000000, -1.000000000000000000 ) ) ;
#16435 = CARTESIAN_POINT ( 'NONE',  ( -14.25622733613999849, 13.93375672974000068, -0.4335075757610999947 ) ) ;
#16436 = CARTESIAN_POINT ( 'NONE',  ( 15.39393908531000044, -10.10652924631000005, 1.349470982713999900 ) ) ;
#16437 = CARTESIAN_POINT ( 'NONE',  ( 18.66008262533330964, 9.600337245201069791, 4.090230547807212069 ) ) ;
#16438 = PRODUCT_DEFINITION_CONTEXT ( 'detailed design', #1066, 'design' ) ;
#16439 = EDGE_CURVE ( 'NONE', #20267, #5409, #23139, .T. ) ;
#16440 = CARTESIAN_POINT ( 'NONE',  ( 44.70988823752291097, 36.26856778792605240, -6.000000000000000000 ) ) ;
#16441 = CARTESIAN_POINT ( 'NONE',  ( 1.633551575390000288, 29.03387112891999777, -1.399019918242000005 ) ) ;
#16442 = CARTESIAN_POINT ( 'NONE',  ( 4.750000000000000000, 17.00000000000000000, 0.000000000000000000 ) ) ;
#16443 = CARTESIAN_POINT ( 'NONE',  ( 13.49999999999999822, -9.438739345711907092, -1.583349858395037835 ) ) ;
#16444 = AXIS2_PLACEMENT_3D ( 'NONE', #22609, #22726, #15461 ) ;
#16445 = VERTEX_POINT ( 'NONE', #17620 ) ;
#16446 = DIRECTION ( 'NONE',  ( 0.000000000000000000, 0.9995313430878892680, -0.03061199413497965940 ) ) ;
#16447 = CARTESIAN_POINT ( 'NONE',  ( 23.84263236754999937, 10.83869278701999939, -3.393613122837999985 ) ) ;
#16448 = CARTESIAN_POINT ( 'NONE',  ( 8.124934037954998800, 12.44999999999999929, 0.000000000000000000 ) ) ;
#16449 = FACE_BOUND ( 'NONE', #12689, .T. ) ;
#16450 = DIRECTION ( 'NONE',  ( 0.000000000000000000, -1.000000000000000000, 0.000000000000000000 ) ) ;
#16451 = CARTESIAN_POINT ( 'NONE',  ( -1.986170008003000698, 11.69253133399998745, 4.555489092804997142 ) ) ;
#16452 = CARTESIAN_POINT ( 'NONE',  ( 1.948101474242260878, 29.06061311738025665, -0.9327975164393527141 ) ) ;
#16453 = EDGE_CURVE ( 'NONE', #23527, #20342, #13984, .T. ) ;
#16454 = CARTESIAN_POINT ( 'NONE',  ( -22.64492594945000192, -10.12459746114000048, -4.604741694910000405 ) ) ;
#16455 = ORIENTED_EDGE ( 'NONE', *, *, #4339, .T. ) ;
#16456 = CARTESIAN_POINT ( 'NONE',  ( 10.35615758860000035, 0.000000000000000000, -7.000000000000000000 ) ) ;
#16457 = ORIENTED_EDGE ( 'NONE', *, *, #22692, .T. ) ;
#16458 = CARTESIAN_POINT ( 'NONE',  ( 1.401975630126000016, 24.25382637699000199, -1.644844636836000129 ) ) ;
#16459 = CARTESIAN_POINT ( 'NONE',  ( 5.316076279024001039, 13.97452196382998579, 3.340701199846999092 ) ) ;
#16460 = AXIS2_PLACEMENT_3D ( 'NONE', #5381, #7185, #12769 ) ;
#16461 = CARTESIAN_POINT ( 'NONE',  ( 12.52688711657000020, -6.216878364870000340, -12.50000000000000000 ) ) ;
#16462 = CONICAL_SURFACE ( 'NONE', #12991, 1.449999902385000095, 0.7853981633972997312 ) ;
#16463 = DIRECTION ( 'NONE',  ( 0.000000000000000000, 1.000000000000000000, 0.000000000000000000 ) ) ;
#16464 = DIRECTION ( 'NONE',  ( 0.000000000000000000, -1.000000000000000000, 0.000000000000000000 ) ) ;
#16465 = ADVANCED_FACE ( 'NONE', ( #15421 ), #6907, .T. ) ;
#16466 = CARTESIAN_POINT ( 'NONE',  ( 12.21300158531000157, -1.561560366126000021, -9.991316461899998558 ) ) ;
#16467 = VERTEX_POINT ( 'NONE', #17495 ) ;
#16468 = DIRECTION ( 'NONE',  ( 0.000000000000000000, 1.000000000000000000, 0.000000000000000000 ) ) ;
#16469 = FACE_OUTER_BOUND ( 'NONE', #10885, .T. ) ;
#16470 = FACE_OUTER_BOUND ( 'NONE', #2141, .T. ) ;
#16471 = EDGE_CURVE ( 'NONE', #13328, #12183, #18029, .T. ) ;
#16472 = EDGE_LOOP ( 'NONE', ( #11656, #16297, #3578, #20296 ) ) ;
#16473 = LINE ( 'NONE', #1949, #22738 ) ;
#16474 = CARTESIAN_POINT ( 'NONE',  ( -2.139397391632000378, 25.28162034356000021, -0.1494154476599000025 ) ) ;
#16475 = CARTESIAN_POINT ( 'NONE',  ( 14.84742989479702402, 10.04995572500151368, -2.448758008351840765 ) ) ;
#16476 = B_SPLINE_CURVE_WITH_KNOTS ( 'NONE', 3,
 ( #1673, #23476, #14281, #5088, #5202, #12585, #16322, #19970, #8592, #7119, #3391, #8954, #10774, #14509, #14158, #12702, #18274, #20096 ),
 .UNSPECIFIED., .F., .F.,
 ( 4, 2, 2, 2, 2, 2, 2, 2, 4 ),
 ( 0.000000000000000000, 0.1250000000000000000, 0.2500000000000000000, 0.3750000000000000000, 0.5000000000000000000, 0.6250000000000000000, 0.7500000000000000000, 0.8750000000000000000, 1.000000000000000000 ),
 .UNSPECIFIED. ) ;
#16477 = DIRECTION ( 'NONE',  ( -1.000000000000000000, 0.000000000000000000, 0.000000000000000000 ) ) ;
#16478 = CARTESIAN_POINT ( 'NONE',  ( 24.23558897616999985, 6.589873019469000504, 9.188931193771999517 ) ) ;
#16479 = CARTESIAN_POINT ( 'NONE',  ( -0.6993571119973001071, 28.64630814436999984, 1.933477428368000073 ) ) ;
#16480 = CARTESIAN_POINT ( 'NONE',  ( 13.85469833500055614, 8.899865800911998193, 1.702839090396268018 ) ) ;
#16481 = CARTESIAN_POINT ( 'NONE',  ( 0.000000000000000000, 24.65000000000000213, 0.000000000000000000 ) ) ;
#16482 = AXIS2_PLACEMENT_3D ( 'NONE', #3204, #21728, #10346 ) ;
#16483 = AXIS2_PLACEMENT_3D ( 'NONE', #7935, #15185, #5987 ) ;
#16484 = CARTESIAN_POINT ( 'NONE',  ( 0.000000000000000000, 16.94999982584599962, -3.049999825846000157 ) ) ;
#16485 = ADVANCED_FACE ( 'NONE', ( #772 ), #3066, .T. ) ;
#16486 = ORIENTED_EDGE ( 'NONE', *, *, #3368, .F. ) ;
#16487 = FACE_OUTER_BOUND ( 'NONE', #16802, .T. ) ;
#16488 = LINE ( 'NONE', #18433, #11926 ) ;
#16489 = ORIENTED_EDGE ( 'NONE', *, *, #5432, .T. ) ;
#16490 = CARTESIAN_POINT ( 'NONE',  ( 0.000000000000000000, 7.049999902385000183, 0.000000000000000000 ) ) ;
#16491 = CARTESIAN_POINT ( 'NONE',  ( 16.90091666666665304, -2.383329820012265010, -8.867965379002798798 ) ) ;
#16492 = DIRECTION ( 'NONE',  ( 0.5000000000000169864, -0.8660254037844289376, 0.000000000000000000 ) ) ;
#16493 = CIRCLE ( 'NONE', #18826, 12.38248359579000102 ) ;
#16494 = CARTESIAN_POINT ( 'NONE',  ( 13.90364969620000046, -10.56859681273999918, 3.047681783393999755 ) ) ;
#16495 = CARTESIAN_POINT ( 'NONE',  ( -14.78159224757403756, 10.16956135232626579, -2.008721191966370778 ) ) ;
#16496 = CARTESIAN_POINT ( 'NONE',  ( 1.960438172910999866, 27.17462896666999939, -1.812210406530999851 ) ) ;
#16497 = ORIENTED_EDGE ( 'NONE', *, *, #22482, .F. ) ;
#16498 = CIRCLE ( 'NONE', #1033, 11.50000000000000000 ) ;
#16499 = CARTESIAN_POINT ( 'NONE',  ( -12.14186006585000044, 2.782277322838000000, -14.15314130824000038 ) ) ;
#16500 = CARTESIAN_POINT ( 'NONE',  ( 13.49999999999999822, 4.107543256433543455, 9.382311906318680172 ) ) ;
#16501 = CARTESIAN_POINT ( 'NONE',  ( 0.3463667137627760018, 28.20780860099773335, -4.418706525551467479 ) ) ;
#16502 = EDGE_CURVE ( 'NONE', #22006, #1172, #16176, .T. ) ;
#16503 = ORIENTED_EDGE ( 'NONE', *, *, #17664, .T. ) ;
#16504 = EDGE_CURVE ( 'NONE', #379, #3740, #3810, .T. ) ;
#16505 = CARTESIAN_POINT ( 'NONE',  ( 22.61757251664768020, -6.462774339621367048, 8.380718989448364908 ) ) ;
#16506 = B_SPLINE_CURVE_WITH_KNOTS ( 'NONE', 3,
 ( #1431, #3494, #3377, #21538, #8580, #10874, #23335, #16188, #14264, #14611 ),
 .UNSPECIFIED., .F., .F.,
 ( 4, 1, 1, 2, 2, 4 ),
 ( 0.000000000000000000, 0.2499999999999986677, 0.3749999999999980016, 0.4374999999999982236, 0.4999999999999984457, 1.000000000000000000 ),
 .UNSPECIFIED. ) ;
#16507 = DIRECTION ( 'NONE',  ( -1.000000000000000000, 0.000000000000000000, 0.000000000000000000 ) ) ;
#16508 = CARTESIAN_POINT ( 'NONE',  ( 16.00077574048890838, -8.450110195753781639, -5.996695405704878468 ) ) ;
#16509 = CARTESIAN_POINT ( 'NONE',  ( -13.56892309062000201, -9.272801077787999446, -4.451380411803999237 ) ) ;
#16510 = CARTESIAN_POINT ( 'NONE',  ( 0.3478861622692999700, 29.63335247264999950, 2.317001308406999804 ) ) ;
#16511 = AXIS2_PLACEMENT_3D ( 'NONE', #8183, #6716, #6605 ) ;
#16513 = AXIS2_PLACEMENT_3D ( 'NONE', #9561, #1939, #18758 ) ;
#16512 = CARTESIAN_POINT ( 'NONE',  ( -18.64256589945999920, -8.356153348075000764, -6.118136038720999537 ) ) ;
#16514 = CARTESIAN_POINT ( 'NONE',  ( 2.137821094052745341, 29.82197946150706258, -0.3076343826834448403 ) ) ;
#16515 = EDGE_CURVE ( 'NONE', #12867, #4139, #9612, .T. ) ;
#16516 = ORIENTED_EDGE ( 'NONE', *, *, #7422, .T. ) ;
#16517 = CARTESIAN_POINT ( 'NONE',  ( -0.7870591911094999560, 24.47971612415000209, -2.034558558890000146 ) ) ;
#16518 = ADVANCED_FACE ( 'NONE', ( #9014 ), #3217, .T. ) ;
#16519 = CARTESIAN_POINT ( 'NONE',  ( 21.23557079259970948, -10.49101315042518578, 1.100340162171684399 ) ) ;
#16520 = CONICAL_SURFACE ( 'NONE', #13415, 2.849999993810000021, 0.7853981633972997312 ) ;
#16521 = DIRECTION ( 'NONE',  ( 0.000000000000000000, 1.000000000000000000, 0.000000000000000000 ) ) ;
#16522 = EDGE_LOOP ( 'NONE', ( #9027, #2536, #4465, #19577, #20641 ) ) ;
#16523 = DIRECTION ( 'NONE',  ( 0.000000000000000000, -1.000000000000000000, 0.000000000000000000 ) ) ;
#16524 = CARTESIAN_POINT ( 'NONE',  ( -14.25851234391999967, -6.965719916941000456, -12.06765612833000034 ) ) ;
#16525 = CARTESIAN_POINT ( 'NONE',  ( 4.782053000032003176, 12.48037919467000378, -0.1093042574499999697 ) ) ;
#16526 = ORIENTED_EDGE ( 'NONE', *, *, #9413, .T. ) ;
#16527 = CARTESIAN_POINT ( 'NONE',  ( 14.46356375731000021, 0.7465905146449000052, 9.123040730097999429 ) ) ;
#16528 = ORIENTED_EDGE ( 'NONE', *, *, #22945, .T. ) ;
#16529 = B_SPLINE_CURVE_WITH_KNOTS ( 'NONE', 3,
 ( #1715, #18768, #2178, #5698, #9338, #20248, #1834, #356, #13084, #14892, #23867, #7637, #18545, #1952, #22283, #10927, #3654, #16710 ),
 .UNSPECIFIED., .F., .F.,
 ( 4, 2, 2, 2, 2, 2, 2, 2, 4 ),
 ( 0.000000000000000000, 0.1250000000000000000, 0.2500000000000000000, 0.3750000000000000000, 0.5000000000000000000, 0.6250000000000000000, 0.7500000000000000000, 0.8750000000000000000, 1.000000000000000000 ),
 .UNSPECIFIED. ) ;
#16530 = CARTESIAN_POINT ( 'NONE',  ( -5.140663980495288499, 15.95621494436533183, 3.330719948904278471 ) ) ;
#16531 = CARTESIAN_POINT ( 'NONE',  ( -14.49999964368427641, -0.5192523986907622291, -12.50000205182226942 ) ) ;
#16532 = ORIENTED_EDGE ( 'NONE', *, *, #2301, .T. ) ;
#16533 = TOROIDAL_SURFACE ( 'NONE', #18097, 10.69999999999999929, 0.8000000000000000444 ) ;
#16534 = CARTESIAN_POINT ( 'NONE',  ( 22.55162270046334072, -4.658593254882972268, -8.082476209181939097 ) ) ;
#16535 = CARTESIAN_POINT ( 'NONE',  ( -25.29471151901000070, -3.100331240559000001, -8.843271378586997855 ) ) ;
#16536 = CARTESIAN_POINT ( 'NONE',  ( 12.04708237236350321, -8.300001990989077427, -10.62407327360604903 ) ) ;
#16537 = DIRECTION ( 'NONE',  ( -1.000000000000000000, 0.000000000000000000, 0.000000000000000000 ) ) ;
#16538 = CARTESIAN_POINT ( 'NONE',  ( -23.46959048080880450, -2.571725778583679123, 10.26703556566396358 ) ) ;
#16539 = CARTESIAN_POINT ( 'NONE',  ( 1.348160915820032946, 27.51919870340391938, -1.702933945497973722 ) ) ;
#16540 = CARTESIAN_POINT ( 'NONE',  ( -6.895677774260998483, 15.29532879160001002, 2.228068349403999893 ) ) ;
#16541 = CARTESIAN_POINT ( 'NONE',  ( 2.022753006592888259, 30.64948983276336136, -0.7574018599443589350 ) ) ;
#16542 = ORIENTED_EDGE ( 'NONE', *, *, #8685, .T. ) ;
#16543 = CARTESIAN_POINT ( 'NONE',  ( 3.546651244991242180, 14.29878692723004008, 4.995327959777049465 ) ) ;
#16544 = CARTESIAN_POINT ( 'NONE',  ( 5.125153960889105242, 13.67047962957576779, -4.635569058280919030 ) ) ;
#16545 = VECTOR ( 'NONE', #22714, 1000.000000000000114 ) ;
#16546 = CARTESIAN_POINT ( 'NONE',  ( -24.39296691846460519, -5.087329382176355885, -9.307667590984573636 ) ) ;
#16547 = CARTESIAN_POINT ( 'NONE',  ( 1.679993844339999987, 27.52771896306000343, -1.552970335759000120 ) ) ;
#16548 = B_SPLINE_CURVE_WITH_KNOTS ( 'NONE', 3,
 ( #4345, #10045, #21179, #18878 ),
 .UNSPECIFIED., .F., .F.,
 ( 4, 4 ),
 ( 0.000000000000000000, 1.000000000000000000 ),
 .UNSPECIFIED. ) ;
#16549 = DIRECTION ( 'NONE',  ( 0.000000000000000000, 0.000000000000000000, 1.000000000000000000 ) ) ;
#16550 = CARTESIAN_POINT ( 'NONE',  ( 4.341046485804971766, 12.26343790180346538, 2.152316017657149860 ) ) ;
#16551 = EDGE_LOOP ( 'NONE', ( #19641, #12402, #660, #23603 ) ) ;
#16552 = CONICAL_SURFACE ( 'NONE', #17332, 9.161549281532000322, 0.02565634000431304615 ) ;
#16553 = ORIENTED_CLOSED_SHELL ( 'NONE', *, #7696, .F. );
#16554 = CARTESIAN_POINT ( 'NONE',  ( -3.593739972392233639, 12.02247931475103471, -3.238798760568094348 ) ) ;
#16555 = CYLINDRICAL_SURFACE ( 'NONE', #19229, 2.500000000000000000 ) ;
#16556 = CARTESIAN_POINT ( 'NONE',  ( 0.000000000000000000, 9.000000000000000000, 0.000000000000000000 ) ) ;
#16557 = EDGE_LOOP ( 'NONE', ( #13108, #18734 ) ) ;
#16558 = CARTESIAN_POINT ( 'NONE',  ( 16.80728936713000365, -9.102589883624000677, 0.000000000000000000 ) ) ;
#16559 = CIRCLE ( 'NONE', #20429, 1.500000000000001332 ) ;
#16560 = CARTESIAN_POINT ( 'NONE',  ( 17.80706408530999951, 3.725969113535000155, -9.559170675091001712 ) ) ;
#16561 = CARTESIAN_POINT ( 'NONE',  ( 18.71397797831778576, 8.679856506646080661, 5.781186714009264094 ) ) ;
#16562 = CARTESIAN_POINT ( 'NONE',  ( 4.000000000000071942, 28.20197603011810372, 1.905018119031321566 ) ) ;
#16563 = DIRECTION ( 'NONE',  ( -1.000000000000000000, 0.000000000000000000, 0.000000000000000000 ) ) ;
#16564 = DIRECTION ( 'NONE',  ( 0.000000000000000000, 1.000000000000000000, 0.000000000000000000 ) ) ;
#16565 = CARTESIAN_POINT ( 'NONE',  ( 13.50000000000000355, -7.263987176282556746, 7.058588360321458310 ) ) ;
#16566 = B_SPLINE_CURVE_WITH_KNOTS ( 'NONE', 3,
 ( #22044, #5453, #20118, #3527, #20230, #1815, #15976, #23369, #18752, #3872, #7491, #104, #7739, #15222, #2048, #16579, #9438, #337 ),
 .UNSPECIFIED., .F., .F.,
 ( 4, 2, 2, 2, 2, 2, 2, 2, 4 ),
 ( 0.000000000000000000, 0.1249999999999999445, 0.2499999999999998890, 0.3749999999999998335, 0.4999999999999997780, 0.6249999999999997780, 0.7499999999999998890, 0.8750000000000000000, 1.000000000000000000 ),
 .UNSPECIFIED. ) ;
#16567 = ORIENTED_EDGE ( 'NONE', *, *, #6981, .F. ) ;
#16568 = CARTESIAN_POINT ( 'NONE',  ( 0.000000000000000000, 26.50000000000000355, 0.000000000000000000 ) ) ;
#16569 = CARTESIAN_POINT ( 'NONE',  ( 23.22869142897999950, -10.53159633789999994, 2.444661321055999981 ) ) ;
#16570 = MANIFOLD_SOLID_BREP ( 'Stock-MAS-673-1', #336 ) ;
#16571 = AXIS2_PLACEMENT_3D ( 'NONE', #10759, #3495, #12571 ) ;
#16572 = CARTESIAN_POINT ( 'NONE',  ( -24.25991043033701544, 10.09239344780629288, 0.3498110921733544876 ) ) ;
#16573 = DIRECTION ( 'NONE',  ( 0.000000000000000000, 1.000000000000000000, 0.000000000000000000 ) ) ;
#16574 = FACE_OUTER_BOUND ( 'NONE', #17965, .T. ) ;
#16575 = CARTESIAN_POINT ( 'NONE',  ( -4.784077338775003518, 12.40247651101999615, 0.7311471882772000441 ) ) ;
#16576 = CARTESIAN_POINT ( 'NONE',  ( -1.261798464217251281, 29.28330482960407721, -1.753041514665990785 ) ) ;
#16577 = DIRECTION ( 'NONE',  ( 0.000000000000000000, -1.000000000000000000, 0.000000000000000000 ) ) ;
#16578 = ORIENTED_EDGE ( 'NONE', *, *, #2299, .T. ) ;
#16579 = CARTESIAN_POINT ( 'NONE',  ( -1.953336881554591065, 23.67957374523190239, 1.002735915203931683 ) ) ;
#16580 = CONICAL_SURFACE ( 'NONE', #3815, 4.309401076758999416, 1.119376321708719590 ) ;
#16581 = ORIENTED_EDGE ( 'NONE', *, *, #18300, .F. ) ;
#16582 = ADVANCED_FACE ( 'NONE', ( #12649 ), #20606, .F. ) ;
#16583 = CARTESIAN_POINT ( 'NONE',  ( 6.273481336118004847, 13.70231772578000573, -0.06242386448472003746 ) ) ;
#16584 = CARTESIAN_POINT ( 'NONE',  ( 11.59051697471118558, 3.660525265870015144, -12.49991113090446149 ) ) ;
#16585 = CARTESIAN_POINT ( 'NONE',  ( 0.000000000000000000, 13.00000000000000000, 0.000000000000000000 ) ) ;
#16586 = SPHERICAL_SURFACE ( 'NONE', #2996, 12.50000000000000000 ) ;
#16587 = CARTESIAN_POINT ( 'NONE',  ( 18.16256424931000168, 7.359336859262000097, -7.874515470102998904 ) ) ;
#16588 =( NAMED_UNIT ( * ) SI_UNIT ( $, .STERADIAN. ) SOLID_ANGLE_UNIT ( ) );
#16589 = ORIENTED_EDGE ( 'NONE', *, *, #946, .F. ) ;
#16590 = CARTESIAN_POINT ( 'NONE',  ( -15.55485259867999837, 4.780789984251000213, 8.479691756156000793 ) ) ;
#16591 = VECTOR ( 'NONE', #7447, 1000.000000000000000 ) ;
#16592 = DIRECTION ( 'NONE',  ( 0.000000000000000000, 0.000000000000000000, -1.000000000000000000 ) ) ;
#16593 = PLANE ( 'NONE',  #3643 ) ;
#16594 = EDGE_LOOP ( 'NONE', ( #15326, #19610, #1926, #5443 ) ) ;
#16595 = EDGE_CURVE ( 'NONE', #3987, #19046, #16473, .T. ) ;
#16596 = CARTESIAN_POINT ( 'NONE',  ( -22.73347842219999748, -8.487330385069000727, -7.414930595396000079 ) ) ;
#16597 = CARTESIAN_POINT ( 'NONE',  ( 1.932058739753999888, 24.83333254276000090, 0.9308572216049000314 ) ) ;
#16598 = CARTESIAN_POINT ( 'NONE',  ( 14.42291159610915408, -1.391709837791132109, -10.22364117141589368 ) ) ;
#16599 = CIRCLE ( 'NONE', #10024, 4.649999999999999467 ) ;
#16600 = LINE ( 'NONE', #20593, #9487 ) ;
#16601 = CARTESIAN_POINT ( 'NONE',  ( 22.40011934649999858, 7.222069075570000329, 8.635347600991998718 ) ) ;
#16602 = CARTESIAN_POINT ( 'NONE',  ( -0.9763371410079000334, 29.33077125539000107, 2.149176381922999646 ) ) ;
#16603 = CARTESIAN_POINT ( 'NONE',  ( 13.80184222826903806, 9.025291706593257857, 0.005214362689862574347 ) ) ;
#16604 = CARTESIAN_POINT ( 'NONE',  ( -3.195009042999999771, 12.10691817796999636, -3.616280525526001988 ) ) ;
#16605 = CARTESIAN_POINT ( 'NONE',  ( -1.615659476414179396, 26.36314323815835792, 1.591840916758156199 ) ) ;
#16606 = TOROIDAL_SURFACE ( 'NONE', #12749, 9.651424765286998664, 0.1000000000000000056 ) ;
#16607 = ORIENTED_EDGE ( 'NONE', *, *, #19335, .F. ) ;
#16608 = CARTESIAN_POINT ( 'NONE',  ( 24.50000000000000355, -10.16681666949672191, 1.404953793027732933 ) ) ;
#16609 = VECTOR ( 'NONE', #18052, 1000.000000000000000 ) ;
#16610 = AXIS2_PLACEMENT_3D ( 'NONE', #9312, #18287, #9194 ) ;
#16611 = ORIENTED_EDGE ( 'NONE', *, *, #16285, .F. ) ;
#16612 = EDGE_CURVE ( 'NONE', #19046, #11394, #16295, .T. ) ;
#16613 = CARTESIAN_POINT ( 'NONE',  ( 11.47028936713000036, -8.379193606113998882, -3.189305674207999708 ) ) ;
#16614 = CARTESIAN_POINT ( 'NONE',  ( -6.249993692867000128, 16.07374114947999999, -3.420978559755999626 ) ) ;
#16615 = DIRECTION ( 'NONE',  ( 0.000000000000000000, 0.8075558440518585401, 0.5897911144953695839 ) ) ;
#16616 = CARTESIAN_POINT ( 'NONE',  ( 18.38109284136999833, 6.121338008679999554, -9.285840504967000086 ) ) ;
#16617 = DIRECTION ( 'NONE',  ( 0.000000000000000000, 0.000000000000000000, -1.000000000000000000 ) ) ;
#16618 = CARTESIAN_POINT ( 'NONE',  ( -2.096579189799000265, 27.56462896666999995, 1.652809762273000027 ) ) ;
#16619 = ORIENTED_EDGE ( 'NONE', *, *, #5666, .F. ) ;
#16620 = CARTESIAN_POINT ( 'NONE',  ( -10.51270006584999805, 9.971762425829000520, -11.02822693349000005 ) ) ;
#16621 = DIRECTION ( 'NONE',  ( -0.5000000000000169864, 0.000000000000000000, 0.8660254037844288266 ) ) ;
#16622 = CARTESIAN_POINT ( 'NONE',  ( -14.48092005499817425, -11.66846015894605770, -4.789644024572045744 ) ) ;
#16623 = VERTEX_POINT ( 'NONE', #22279 ) ;
#16624 = EDGE_CURVE ( 'NONE', #6263, #16291, #12325, .T. ) ;
#16625 = CARTESIAN_POINT ( 'NONE',  ( -12.26714646669999986, 6.430159825535999296, -13.55186498671000095 ) ) ;
#16626 = CARTESIAN_POINT ( 'NONE',  ( 20.81320603379664647, -2.409608536984290783, -8.965749368246138218 ) ) ;
#16627 = CYLINDRICAL_SURFACE ( 'NONE', #16460, 4.750000000000000000 ) ;
#16628 = CARTESIAN_POINT ( 'NONE',  ( 16.01310729382478826, -8.177487985005738480, -6.358481180217821382 ) ) ;
#16629 = CARTESIAN_POINT ( 'NONE',  ( -14.29157635075000066, 5.124190584818000715, 9.732655983376998776 ) ) ;
#16630 = CARTESIAN_POINT ( 'NONE',  ( -2.328322743135000206, 31.00015586545000090, -0.2610490293201000456 ) ) ;
#16631 = AXIS2_PLACEMENT_3D ( 'NONE', #22248, #11720, #19095 ) ;
#16632 = CARTESIAN_POINT ( 'NONE',  ( -18.84569624743000205, -10.33415972889999956, 0.7423446255362999846 ) ) ;
#16633 = ADVANCED_FACE ( 'NONE', ( #7271 ), #17310, .F. ) ;
#16634 = CARTESIAN_POINT ( 'NONE',  ( 2.093433345533683099, 29.77039470201872717, 0.5628675214677475447 ) ) ;
#16635 = ORIENTED_EDGE ( 'NONE', *, *, #13375, .T. ) ;
#16636 = CARTESIAN_POINT ( 'NONE',  ( 1.585875242673999930, 25.49199905389999898, 1.504396160838000096 ) ) ;
#16637 = CARTESIAN_POINT ( 'NONE',  ( 19.56154115649750835, -9.843004022036630829, -3.930645473631872555 ) ) ;
#16638 = CARTESIAN_POINT ( 'NONE',  ( -0.8685634062544059786, 23.64940451091839790, -1.966097736889167225 ) ) ;
#16639 = EDGE_LOOP ( 'NONE', ( #17745, #23074, #22194, #20231 ) ) ;
#16640 = EDGE_CURVE ( 'NONE', #9734, #386, #6476, .T. ) ;
#16641 = CARTESIAN_POINT ( 'NONE',  ( 0.000000000000000000, 16.89999999999999858, -3.000000000000013323 ) ) ;
#16642 = FACE_OUTER_BOUND ( 'NONE', #12786, .T. ) ;
#16643 = EDGE_CURVE ( 'NONE', #22477, #15451, #5327, .T. ) ;
#16644 = CARTESIAN_POINT ( 'NONE',  ( -0.5922303555482001380, 11.50778550622999852, -4.771349591085003006 ) ) ;
#16645 = CARTESIAN_POINT ( 'NONE',  ( 12.48918875731000000, 5.414613097170000167, 7.315858880121999697 ) ) ;
#16646 = VERTEX_POINT ( 'NONE', #15119 ) ;
#16647 = CARTESIAN_POINT ( 'NONE',  ( -4.645659211928634846, 15.61175543958523981, 3.991716869351718433 ) ) ;
#16648 = MANIFOLD_SOLID_BREP ( 'Stock-MAS-673-1', #20088 ) ;
#16649 = CARTESIAN_POINT ( 'NONE',  ( -2.434931691670787934, 29.63333333333333286, 0.6543697108982051702 ) ) ;
#16650 = VERTEX_POINT ( 'NONE', #19120 ) ;
#16651 = ADVANCED_FACE ( 'NONE', ( #4115 ), #5387, .F. ) ;
#16652 = FACE_OUTER_BOUND ( 'NONE', #1096, .T. ) ;
#16653 = ADVANCED_FACE ( 'NONE', ( #466 ), #11528, .F. ) ;
#16654 = CARTESIAN_POINT ( 'NONE',  ( 2.290777621496001171, 11.89229473561999839, 4.253142527875998447 ) ) ;
#16655 = AXIS2_PLACEMENT_3D ( 'NONE', #10314, #10677, #14419 ) ;
#16656 = CARTESIAN_POINT ( 'NONE',  ( -22.77885345450999921, 8.335141950908999675, 4.829927459581000448 ) ) ;
#16657 = CARTESIAN_POINT ( 'NONE',  ( -13.93312122640000084, 8.641212754535999352, -2.222119620850000032 ) ) ;
#16658 = CARTESIAN_POINT ( 'NONE',  ( -23.82988224127242205, 8.924282944053008038, 5.705145624228507906 ) ) ;
#16659 = CARTESIAN_POINT ( 'NONE',  ( 1.994114618456069632, 26.41019129450748082, -1.176349860261615143 ) ) ;
#16660 = CARTESIAN_POINT ( 'NONE',  ( 16.03170833333333078, 1.189047888634058303, 9.082686945706512915 ) ) ;
#16661 = DIRECTION ( 'NONE',  ( 0.000000000000000000, 1.000000000000000000, 0.000000000000000000 ) ) ;
#16662 = CARTESIAN_POINT ( 'NONE',  ( 2.141160088383624149, 30.62055634019574057, -0.2848521897935961666 ) ) ;
#16663 = VERTEX_POINT ( 'NONE', #14402 ) ;
#16664 = CARTESIAN_POINT ( 'NONE',  ( 0.7923955384326393236, 26.27095271610905769, 2.035725376479952331 ) ) ;
#16665 = CARTESIAN_POINT ( 'NONE',  ( 14.27789894812851301, 7.165480330777101337, 5.593028109329393871 ) ) ;
#16666 = CARTESIAN_POINT ( 'NONE',  ( -23.64322841789023144, 9.153672998692304219, 5.321353405662923031 ) ) ;
#16667 = CARTESIAN_POINT ( 'NONE',  ( 2.266239109532000029, 26.65021896306000215, -0.3134588398365999451 ) ) ;
#16668 = DIRECTION ( 'NONE',  ( 0.000000000000000000, -1.000000000000000000, 0.000000000000000000 ) ) ;
#16669 = CARTESIAN_POINT ( 'NONE',  ( 3.368441454496569509, 11.95864406845431382, 3.464918207308566700 ) ) ;
#16670 = ORIENTED_EDGE ( 'NONE', *, *, #14566, .F. ) ;
#16671 = CARTESIAN_POINT ( 'NONE',  ( -3.391218646352913701, 11.96540231941397714, -3.439755270211452221 ) ) ;
#16672 = LINE ( 'NONE', #9651, #2214 ) ;
#16673 = CARTESIAN_POINT ( 'NONE',  ( 0.7185112213146519489, 28.67261440401754058, 2.100171626021731797 ) ) ;
#16674 = ORIENTED_EDGE ( 'NONE', *, *, #19165, .T. ) ;
#16675 = ADVANCED_FACE ( 'NONE', ( #1799 ), #9186, .T. ) ;
#16676 = CARTESIAN_POINT ( 'NONE',  ( -1.989999999999999991, 9.799994897958001161, 7.500000000000000000 ) ) ;
#16677 = CARTESIAN_POINT ( 'NONE',  ( 12.54206408531000072, 8.432320343758000547, -5.597842903599000053 ) ) ;
#16678 = CARTESIAN_POINT ( 'NONE',  ( 18.16027265446844297, 2.522309870967282652, -10.13363737170168477 ) ) ;
#16679 = CARTESIAN_POINT ( 'NONE',  ( -23.99212502906159017, 5.142273543674439118, 12.50000000000264144 ) ) ;
#16680 = CARTESIAN_POINT ( 'NONE',  ( -2.196349052328999907, 29.40402464138999861, -0.8124029318252000698 ) ) ;
#16681 = CARTESIAN_POINT ( 'NONE',  ( 23.99062354302999722, -7.716878364870000340, -11.63397459621999985 ) ) ;
#16682 = CARTESIAN_POINT ( 'NONE',  ( 0.5243867192824805956, 24.49999999999999645, 2.383703889157006373 ) ) ;
#16683 = ORIENTED_EDGE ( 'NONE', *, *, #12170, .F. ) ;
#16684 = CARTESIAN_POINT ( 'NONE',  ( -24.50000000000293454, 10.95355345391266511, 6.027888894412471998 ) ) ;
#16685 = CARTESIAN_POINT ( 'NONE',  ( 23.48853416324000065, 0.4636106205751999720, -11.33838736911999945 ) ) ;
#16686 = CARTESIAN_POINT ( 'NONE',  ( -24.32816120980435670, 9.615500567526682474, -3.310132273745861387 ) ) ;
#16687 = ORIENTED_EDGE ( 'NONE', *, *, #22403, .T. ) ;
#16688 = CARTESIAN_POINT ( 'NONE',  ( 13.63946275288138565, -8.561423039799775481, 5.801876326834510600 ) ) ;
#16689 = CARTESIAN_POINT ( 'NONE',  ( -2.100000000000000089, 18.00000000000000000, 0.000000000000000000 ) ) ;
#16690 = CARTESIAN_POINT ( 'NONE',  ( -4.479356662876004869, 12.28735091408998592, 1.840098238078000881 ) ) ;
#16691 = APPLICATION_CONTEXT ( 'automotive_design' ) ;
#16692 = CARTESIAN_POINT ( 'NONE',  ( 1.930882614817647891, 29.06295433460837430, -0.9682181790307279323 ) ) ;
#16693 = CARTESIAN_POINT ( 'NONE',  ( -20.97408049164000232, -11.05085136034000115, 0.7637451293671000396 ) ) ;
#16694 = VERTEX_POINT ( 'NONE', #5209 ) ;
#16695 = CARTESIAN_POINT ( 'NONE',  ( 8.196152422706999729, 26.90192378864669820, 6.000000000000000000 ) ) ;
#16696 = ORIENTED_EDGE ( 'NONE', *, *, #15458, .F. ) ;
#16697 = CARTESIAN_POINT ( 'NONE',  ( -0.6958892446922999575, 24.01090960993000323, 2.247974813822000151 ) ) ;
#16698 = CARTESIAN_POINT ( 'NONE',  ( 6.181149466256997016, 13.72396362260998970, 1.092410950252000301 ) ) ;
#16699 = CARTESIAN_POINT ( 'NONE',  ( 16.31599770046333120, 1.190002857594358643, 9.089982371172002473 ) ) ;
#16700 = DIRECTION ( 'NONE',  ( 0.000000000000000000, 1.000000000000000000, 0.000000000000000000 ) ) ;
#16701 = DIRECTION ( 'NONE',  ( 0.000000000000000000, 1.000000000000000000, 0.000000000000000000 ) ) ;
#16702 = CARTESIAN_POINT ( 'NONE',  ( 14.18737658531000001, 3.962519675866999602, -9.360324180111000203 ) ) ;
#16703 = CARTESIAN_POINT ( 'NONE',  ( -14.33607051085999906, 5.206569482801000071, -8.184903637703000001 ) ) ;
#16704 = CARTESIAN_POINT ( 'NONE',  ( -14.00000000000000000, 8.507292963980999545, 3.029321241734000303 ) ) ;
#16705 = CARTESIAN_POINT ( 'NONE',  ( -14.44633172591991865, 2.842506014205136822, 12.49999152949037651 ) ) ;
#16706 = VERTEX_POINT ( 'NONE', #12592 ) ;
#16707 = CARTESIAN_POINT ( 'NONE',  ( -10.16281054619604873, 15.91872981196863002, -1.078691087397217752 ) ) ;
#16708 = CARTESIAN_POINT ( 'NONE',  ( 1.645212785078999929, 25.60182591557000009, 1.375746322452999992 ) ) ;
#16709 = CARTESIAN_POINT ( 'NONE',  ( 14.76997825937266740, 9.033527493718441548, -5.004583818473492762 ) ) ;
#16710 = CARTESIAN_POINT ( 'NONE',  ( -18.63376253787999914, -9.149460784975000038, 0.000000000000000000 ) ) ;
#16711 = CARTESIAN_POINT ( 'NONE',  ( 21.48238453167000017, -7.521219210359999963, -8.342195645638000201 ) ) ;
#16712 = EDGE_CURVE ( 'NONE', #2832, #12632, #13281, .T. ) ;
#16713 = CARTESIAN_POINT ( 'NONE',  ( -2.548054378949999865, 29.87161659520999990, -0.1605585572842999909 ) ) ;
#16714 = CARTESIAN_POINT ( 'NONE',  ( 14.13908848849179023, 3.495271894151044556, 8.348058256251976061 ) ) ;
#16715 = CARTESIAN_POINT ( 'NONE',  ( -6.591948041516452861, 15.40797180132708988, -1.571325980949459078 ) ) ;
#16716 = FACE_OUTER_BOUND ( 'NONE', #13948, .T. ) ;
#16717 = CARTESIAN_POINT ( 'NONE',  ( 20.52539899991999661, 5.356978891688999767, 10.06605121447999984 ) ) ;
#16718 = VERTEX_POINT ( 'NONE', #21035 ) ;
#16719 = AXIS2_PLACEMENT_3D ( 'NONE', #23262, #19888, #1480 ) ;
#16720 = CARTESIAN_POINT ( 'NONE',  ( 1.167231323634179585, 23.98248082379630475, -2.207338634965280377 ) ) ;
#16721 = ORIENTED_EDGE ( 'NONE', *, *, #20523, .F. ) ;
#16722 = CARTESIAN_POINT ( 'NONE',  ( -15.65412077250664957, 9.072997304709783606, -1.187525622282732396 ) ) ;
#16723 = DIRECTION ( 'NONE',  ( 0.000000000000000000, 0.000000000000000000, -1.000000000000000000 ) ) ;
#16724 = CARTESIAN_POINT ( 'NONE',  ( 1.125885562883627733, 24.63699083177793625, 1.968842548519072366 ) ) ;
#16725 = CARTESIAN_POINT ( 'NONE',  ( 17.87356944879000054, -6.873864763588999338, -8.725743989736999495 ) ) ;
#16726 = CARTESIAN_POINT ( 'NONE',  ( -6.046835300290999804, 16.30334124114000360, 1.000000020649999932 ) ) ;
#16727 = CARTESIAN_POINT ( 'NONE',  ( 1.206163983883000057, 25.72006359724000291, -2.153772461420000006 ) ) ;
#16728 = EDGE_LOOP ( 'NONE', ( #6299, #1887, #482 ) ) ;
#16729 = ORIENTED_EDGE ( 'NONE', *, *, #21707, .F. ) ;
#16730 = CARTESIAN_POINT ( 'NONE',  ( -10.20723256584999916, 13.42721542333999984, 6.384960544076999867 ) ) ;
#16731 = CARTESIAN_POINT ( 'NONE',  ( 0.7519233154364799443, 6.819034920433882263, -1.581610603952285254 ) ) ;
#16732 = CARTESIAN_POINT ( 'NONE',  ( 1.500000000000000000, 8.900000000000000355, 0.000000000000000000 ) ) ;
#16733 = ORIENTED_EDGE ( 'NONE', *, *, #6745, .T. ) ;
#16734 = CARTESIAN_POINT ( 'NONE',  ( -14.48633706258206111, 10.11155074087842642, 7.486293916575140095 ) ) ;
#16735 = DIRECTION ( 'NONE',  ( -0.000000000000000000, 1.000000000000000000, 0.000000000000000000 ) ) ;
#16736 = AXIS2_PLACEMENT_3D ( 'NONE', #11150, #9565, #7387 ) ;
#16737 = CARTESIAN_POINT ( 'NONE',  ( 6.239308309756287585, 13.68455386514935412, 1.647755693301848456 ) ) ;
#16738 = CARTESIAN_POINT ( 'NONE',  ( 15.90272818354428175, -9.982911839440134827, -2.763178835720944360 ) ) ;
#16739 = CARTESIAN_POINT ( 'NONE',  ( -18.01742253012000106, -2.120327895178999889, 10.89685495860999964 ) ) ;
#16740 = ADVANCED_FACE ( 'NONE', ( #11604, #683 ), #8090, .T. ) ;
#16741 = CARTESIAN_POINT ( 'NONE',  ( 1.435961984585999884, 29.47955444677999992, 1.657103211982000168 ) ) ;
#16742 = CARTESIAN_POINT ( 'NONE',  ( -15.63636876114000351, -8.424167882059999002, 6.770715351507000435 ) ) ;
#16743 = CARTESIAN_POINT ( 'NONE',  ( 1.551074172888720959, 29.70570296557802337, 1.503492241676404717 ) ) ;
#16744 = EDGE_LOOP ( 'NONE', ( #12431, #21537, #16721, #15921 ) ) ;
#16745 = CARTESIAN_POINT ( 'NONE',  ( 1.552832420049000017, 24.32177879045000424, -1.744744256400999838 ) ) ;
#16746 = CARTESIAN_POINT ( 'NONE',  ( 19.78852822580074999, -4.133238257719290765, -9.662078402654971754 ) ) ;
#16747 = CARTESIAN_POINT ( 'NONE',  ( -18.10935057530256387, 0.4203439791810718029, 10.44572940319434196 ) ) ;
#16748 = ORIENTED_EDGE ( 'NONE', *, *, #10903, .F. ) ;
#16749 = CARTESIAN_POINT ( 'NONE',  ( -4.012824720309999371, 13.17021387432998658, 4.696499411533000767 ) ) ;
#16750 = EDGE_CURVE ( 'NONE', #2766, #7012, #21189, .T. ) ;
#16751 = PRODUCT_DEFINITION_FORMATION_WITH_SPECIFIED_SOURCE ( 'ANY', '', #483, .NOT_KNOWN. ) ;
#16752 = CARTESIAN_POINT ( 'NONE',  ( -13.99999999999999645, -9.053648303160509059, 5.060582752402400075 ) ) ;
#16753 = CARTESIAN_POINT ( 'NONE',  ( 14.02481375730999957, 9.137735611494999688, -0.2793723515763000265 ) ) ;
#16754 = PRODUCT_DEFINITION_CONTEXT ( 'detailed design', #9733, 'design' ) ;
#16755 = ORIENTED_EDGE ( 'NONE', *, *, #19284, .F. ) ;
#16756 = DIRECTION ( 'NONE',  ( 0.000000000000000000, 0.000000000000000000, 1.000000000000000000 ) ) ;
#16757 = EDGE_CURVE ( 'NONE', #14966, #23789, #20680, .T. ) ;
#16758 = CARTESIAN_POINT ( 'NONE',  ( 18.75008227645999881, 0.000000000000000000, 0.000000000000000000 ) ) ;
#16759 = AXIS2_PLACEMENT_3D ( 'NONE', #16172, #10257, #6856 ) ;
#16760 = ORIENTED_EDGE ( 'NONE', *, *, #20605, .F. ) ;
#16761 = CARTESIAN_POINT ( 'NONE',  ( 22.77837270046333629, 2.422573927148270023, -9.014964020370104691 ) ) ;
#16762 = CARTESIAN_POINT ( 'NONE',  ( 4.699418951522004839, 12.59868348402000748, 0.6614101461372995372 ) ) ;
#16763 = CARTESIAN_POINT ( 'NONE',  ( 12.00000000000000000, 5.273090321616999532, -7.267806174758000282 ) ) ;
#16764 = EDGE_CURVE ( 'NONE', #7987, #2252, #4450, .T. ) ;
#16765 = DIRECTION ( 'NONE',  ( -6.752000474851949799E-22, 1.631346932539999964E-10, -1.000000000000000000 ) ) ;
#16766 = CARTESIAN_POINT ( 'NONE',  ( 2.402140947178999647E-14, 29.00000000000000000, 2.500000000000000000 ) ) ;
#16767 = CARTESIAN_POINT ( 'NONE',  ( -20.99901840903234529, -6.127583174698123081, -8.547554176268754134 ) ) ;
#16768 = CARTESIAN_POINT ( 'NONE',  ( 5.314999799853000972, 13.91584611406999983, 3.802386931276000137 ) ) ;
#16769 = CARTESIAN_POINT ( 'NONE',  ( 0.000000000000000000, 24.40000007355299871, 0.000000000000000000 ) ) ;
#16771 = AXIS2_PLACEMENT_3D ( 'NONE', #22817, #4424, #15431 ) ;
#16770 = CARTESIAN_POINT ( 'NONE',  ( 0.5899383557787000187, 29.08750240009999999, 2.621867217767999581 ) ) ;
#16772 = CARTESIAN_POINT ( 'NONE',  ( -0.6694547791842193618, 30.36376599517464570, 2.053524939800617233 ) ) ;
#16773 = ORIENTED_EDGE ( 'NONE', *, *, #7439, .T. ) ;
#16774 = CARTESIAN_POINT ( 'NONE',  ( 21.72047034351999883, 0.7717287101376000269, 9.798846879612002070 ) ) ;
#16775 = CARTESIAN_POINT ( 'NONE',  ( 14.02900943697788527, 8.904994502184068850, -1.790900335187071590 ) ) ;
#16776 = CARTESIAN_POINT ( 'NONE',  ( -23.18803004254179001, -5.362570460539083150, 9.113462231227742905 ) ) ;
#16777 = CARTESIAN_POINT ( 'NONE',  ( -1.488814495283000028, 27.47864211382000121, -1.743177805438000050 ) ) ;
#16778 = EDGE_CURVE ( 'NONE', #11958, #23264, #22934, .T. ) ;
#16779 = AXIS2_PLACEMENT_3D ( 'NONE', #1481, #5578, #12958 ) ;
#16780 = CIRCLE ( 'NONE', #21837, 16.43375672870000415 ) ;
#16781 = CARTESIAN_POINT ( 'NONE',  ( -2.500000000000000000, 27.19999999999999929, 0.000000000000000000 ) ) ;
#16782 = CARTESIAN_POINT ( 'NONE',  ( 1.004037071924726687, 11.52581781820473239, 4.707233457423458667 ) ) ;
#16783 = VERTEX_POINT ( 'NONE', #16916 ) ;
#16784 = CARTESIAN_POINT ( 'NONE',  ( -3.741193895918689005, 12.06686126286441407, -3.070321243407096112 ) ) ;
#16785 = DIRECTION ( 'NONE',  ( 0.4593435542646316372, -0.8882586893217174762, 0.000000000000000000 ) ) ;
#16786 = CARTESIAN_POINT ( 'NONE',  ( -4.000000000000116351, 27.99999999999975842, 0.3805779584833383633 ) ) ;
#16787 = ORIENTED_EDGE ( 'NONE', *, *, #16643, .T. ) ;
#16788 =( BOUNDED_SURFACE ( )  B_SPLINE_SURFACE ( 3, 3, ( 
 ( #10906, #7025, #16339, #19760, #3287, #10669, #9080, #18290, #14412, #6783, #21804, #10792, #23495, #1587, #16451, #12602, #5105, #1342, #3522, #12486, #19988, #8969, #23730, #23841, #5332, #6908, #22040, #8733, #17936, #14175, #4986, #14526 ),
 ( #12832, #21918, #20113, #12372, #11014, #14301, #18398, #8609, #21693, #15970, #23365, #18057, #3169, #100, #213, #23965, #6024, #4098, #3743, #11376, #13061, #22151, #11259, #7485, #14755, #18748, #3982, #18871, #2277, #9670, #17051, #18638 ),
 ( #13410, #14870, #16805, #448, #2044, #16575, #20811, #22257, #16690, #5562, #7735, #11133, #1929, #22616, #12939, #4221, #9434, #7851, #5673, #20457, #11494, #3868, #7607, #20336, #11614, #13179, #5905, #14985, #22382, #5796, #15218, #20568 ),
 ( #1809, #7371, #2158, #15101, #9197, #18519, #9550, #9316, #16928, #331, #22496, #13291, #20690, #23090, #6267, #9784, #2643, #15584, #4584, #11977, #21047, #22854, #10039, #22732, #8101, #6147, #694, #17423, #21172, #13650, #817, #15343 ),
 ( #13771, #15700, #13536, #19363, #7971, #15468, #2769, #8218, #4460, #17540, #19230, #20931, #11850, #22971, #6514, #10155, #6388, #8334, #935, #18984, #2395, #17170, #565, #4337, #11729, #19103, #2515, #9905, #17293, #18948, #15298, #7692 ),
 ( #2006, #18828, #9627, #171, #2355, #7810, #5752, #5871, #14941, #15066, #14824, #20892, #9746, #18599, #2234, #3944, #13015, #2117, #22337, #5632, #17011, #410, #17132, #527, #7930, #22689, #9508, #20416, #16762, #3824, #6099, #9390 ),
 ( #7443, #11688, #13142, #7562, #11221, #22577, #20535, #11339, #13491, #18709, #4298, #16883, #19062, #291, #22460, #2476, #13256, #20649, #4058, #16654, #11453, #20767, #15182, #58, #22217, #5983, #13366, #4176, #11571, #2595, #21258, #6471 ) ),
 .UNSPECIFIED., .F., .F., .T. ) 
 B_SPLINE_SURFACE_WITH_KNOTS ( ( 4, 3, 4 ),
 ( 4, 1, 1, 1, 1, 1, 1, 1, 1, 1, 1, 1, 1, 1, 1, 1, 1, 1, 1, 1, 1, 1, 1, 1, 1, 1, 1, 1, 1, 4 ),
 ( 0.000000000000000000, 1.000000000000000000, 2.000000000000000000 ),
 ( -0.0001618831681000999832, 0.000000000000000000, 0.008762561342867999925, 0.01824509674601000261, 0.02863315657921999824, 0.04005085953976000174, 0.05263615618096000037, 0.06652419853735000443, 0.08184912555068998841, 0.09881173633437000114, 0.1176787978263000023, 0.1387116773469999897, 0.1621789585680999957, 0.1887288111371999977, 0.2191170703197999892, 0.2517299998975999764, 0.2825862214344000423, 0.3099915928082999650, 0.3345416994503000452, 0.3566258367156999731, 0.3765620894444000055, 0.3945985271376999948, 0.4110154862469999615, 0.4260441420834000237, 0.4400513890198000100, 0.4540949684832999989, 0.4686848077695999759, 0.4831735293021999778, 0.4971812856050999985, 0.5099256701170999939 ),
 .UNSPECIFIED. ) 
 GEOMETRIC_REPRESENTATION_ITEM ( )  RATIONAL_B_SPLINE_SURFACE ( (
 ( 1.293520787057000021, 1.293520787057000021, 1.293520787057000021, 1.293520787057000021, 1.293520787057000021, 1.293520787057000021, 1.293520787057000021, 1.293520787057000021, 1.293520787057000021, 1.293520787057000021, 1.293520787057000021, 1.293520787057000021, 1.293520787057000021, 1.293520787057000021, 1.293520787057000021, 1.293520787057000021, 1.293520787057000021, 1.293520787057000021, 1.293520787057000021, 1.293520787057000021, 1.293520787057000021, 1.293520787057000021, 1.293520787057000021, 1.293520787057000021, 1.293520787057000021, 1.293520787057000021, 1.293520787057000021, 1.293520787057000021, 1.293520787057000021, 1.293520787057000021, 1.293520787057000021, 1.293520787057000021),
 ( 0.9021597376475999353, 0.9021597376475999353, 0.9021597376475999353, 0.9021597376475999353, 0.9021597376475999353, 0.9021597376475999353, 0.9021597376475999353, 0.9021597376475999353, 0.9021597376475999353, 0.9021597376475999353, 0.9021597376475999353, 0.9021597376475999353, 0.9021597376475999353, 0.9021597376475999353, 0.9021597376475999353, 0.9021597376475999353, 0.9021597376475999353, 0.9021597376475999353, 0.9021597376475999353, 0.9021597376475999353, 0.9021597376475999353, 0.9021597376475999353, 0.9021597376475999353, 0.9021597376475999353, 0.9021597376475999353, 0.9021597376475999353, 0.9021597376475999353, 0.9021597376475999353, 0.9021597376475999353, 0.9021597376475999353, 0.9021597376475999353, 0.9021597376475999353),
 ( 0.9021597376475999353, 0.9021597376475999353, 0.9021597376475999353, 0.9021597376475999353, 0.9021597376475999353, 0.9021597376475999353, 0.9021597376475999353, 0.9021597376475999353, 0.9021597376475999353, 0.9021597376475999353, 0.9021597376475999353, 0.9021597376475999353, 0.9021597376475999353, 0.9021597376475999353, 0.9021597376475999353, 0.9021597376475999353, 0.9021597376475999353, 0.9021597376475999353, 0.9021597376475999353, 0.9021597376475999353, 0.9021597376475999353, 0.9021597376475999353, 0.9021597376475999353, 0.9021597376475999353, 0.9021597376475999353, 0.9021597376475999353, 0.9021597376475999353, 0.9021597376475999353, 0.9021597376475999353, 0.9021597376475999353, 0.9021597376475999353, 0.9021597376475999353),
 ( 1.293520787057000021, 1.293520787057000021, 1.293520787057000021, 1.293520787057000021, 1.293520787057000021, 1.293520787057000021, 1.293520787057000021, 1.293520787057000021, 1.293520787057000021, 1.293520787057000021, 1.293520787057000021, 1.293520787057000021, 1.293520787057000021, 1.293520787057000021, 1.293520787057000021, 1.293520787057000021, 1.293520787057000021, 1.293520787057000021, 1.293520787057000021, 1.293520787057000021, 1.293520787057000021, 1.293520787057000021, 1.293520787057000021, 1.293520787057000021, 1.293520787057000021, 1.293520787057000021, 1.293520787057000021, 1.293520787057000021, 1.293520787057000021, 1.293520787057000021, 1.293520787057000021, 1.293520787057000021),
 ( 0.9021597376475999353, 0.9021597376475999353, 0.9021597376475999353, 0.9021597376475999353, 0.9021597376475999353, 0.9021597376475999353, 0.9021597376475999353, 0.9021597376475999353, 0.9021597376475999353, 0.9021597376475999353, 0.9021597376475999353, 0.9021597376475999353, 0.9021597376475999353, 0.9021597376475999353, 0.9021597376475999353, 0.9021597376475999353, 0.9021597376475999353, 0.9021597376475999353, 0.9021597376475999353, 0.9021597376475999353, 0.9021597376475999353, 0.9021597376475999353, 0.9021597376475999353, 0.9021597376475999353, 0.9021597376475999353, 0.9021597376475999353, 0.9021597376475999353, 0.9021597376475999353, 0.9021597376475999353, 0.9021597376475999353, 0.9021597376475999353, 0.9021597376475999353),
 ( 0.9021597376475999353, 0.9021597376475999353, 0.9021597376475999353, 0.9021597376475999353, 0.9021597376475999353, 0.9021597376475999353, 0.9021597376475999353, 0.9021597376475999353, 0.9021597376475999353, 0.9021597376475999353, 0.9021597376475999353, 0.9021597376475999353, 0.9021597376475999353, 0.9021597376475999353, 0.9021597376475999353, 0.9021597376475999353, 0.9021597376475999353, 0.9021597376475999353, 0.9021597376475999353, 0.9021597376475999353, 0.9021597376475999353, 0.9021597376475999353, 0.9021597376475999353, 0.9021597376475999353, 0.9021597376475999353, 0.9021597376475999353, 0.9021597376475999353, 0.9021597376475999353, 0.9021597376475999353, 0.9021597376475999353, 0.9021597376475999353, 0.9021597376475999353),
 ( 1.293520787057000021, 1.293520787057000021, 1.293520787057000021, 1.293520787057000021, 1.293520787057000021, 1.293520787057000021, 1.293520787057000021, 1.293520787057000021, 1.293520787057000021, 1.293520787057000021, 1.293520787057000021, 1.293520787057000021, 1.293520787057000021, 1.293520787057000021, 1.293520787057000021, 1.293520787057000021, 1.293520787057000021, 1.293520787057000021, 1.293520787057000021, 1.293520787057000021, 1.293520787057000021, 1.293520787057000021, 1.293520787057000021, 1.293520787057000021, 1.293520787057000021, 1.293520787057000021, 1.293520787057000021, 1.293520787057000021, 1.293520787057000021, 1.293520787057000021, 1.293520787057000021, 1.293520787057000021) ) ) 
 REPRESENTATION_ITEM ( '' )  SURFACE ( )  );
#16789 = DIRECTION ( 'NONE',  ( 0.000000000000000000, -0.4408793407386908947, 0.8975663802247817458 ) ) ;
#16790 = CARTESIAN_POINT ( 'NONE',  ( 18.24581408530999838, 9.747919580236001025, 3.236577786812999680 ) ) ;
#16791 = CARTESIAN_POINT ( 'NONE',  ( 18.06410204184560797, -0.9209652123333776919, -10.37059875417824095 ) ) ;
#16792 = ADVANCED_FACE ( 'NONE', ( #5785 ), #18860, .T. ) ;
#16793 = CARTESIAN_POINT ( 'NONE',  ( 3.999709959623201971, 28.03198827073818933, 0.7544996413140969693 ) ) ;
#16794 = CARTESIAN_POINT ( 'NONE',  ( 2.112683224871000132, 28.96769140845000123, -0.4028931246161000512 ) ) ;
#16795 = ADVANCED_FACE ( 'NONE', ( #11839 ), #11177, .T. ) ;
#16796 = CARTESIAN_POINT ( 'NONE',  ( 17.56239037306000128, -5.826923919702999832, 9.176156247568000524 ) ) ;
#16797 = CARTESIAN_POINT ( 'NONE',  ( 7.278495274186999708, 27.32666689084959799, 6.000000000000000000 ) ) ;
#16798 = EDGE_LOOP ( 'NONE', ( #23904, #615, #4733, #4388 ) ) ;
#16799 = CARTESIAN_POINT ( 'NONE',  ( -1.536366799937273875, 28.91666666666665719, 1.999167105995461213 ) ) ;
#16800 = CARTESIAN_POINT ( 'NONE',  ( 22.52049502035999851, 9.667974779076999425, 4.796159037922000046 ) ) ;
#16801 = CARTESIAN_POINT ( 'NONE',  ( -8.099999999999999645, 10.59999999999999964, 0.000000000000000000 ) ) ;
#16802 = EDGE_LOOP ( 'NONE', ( #7927, #13505, #22650, #6910, #21920, #18697 ) ) ;
#16803 = CARTESIAN_POINT ( 'NONE',  ( 11.33972984855999933, -8.487386343340000749, -2.878673876759000105 ) ) ;
#16804 = CARTESIAN_POINT ( 'NONE',  ( -10.04281598263999875, 20.50000000000000000, 1.000000000000000000 ) ) ;
#16805 = CARTESIAN_POINT ( 'NONE',  ( -4.836297190787002265, 12.42285795213999755, -0.06016108829675999997 ) ) ;
#16806 = CARTESIAN_POINT ( 'NONE',  ( 1.964204535412830577, 29.05835064317297523, -0.8983286665718945851 ) ) ;
#16807 = CARTESIAN_POINT ( 'NONE',  ( -24.31577140724999708, -6.742003853025999582, -8.902789307808999908 ) ) ;
#16808 = ORIENTED_EDGE ( 'NONE', *, *, #10234, .T. ) ;
#16809 = ADVANCED_FACE ( 'NONE', ( #2147 ), #9539, .T. ) ;
#16810 = EDGE_CURVE ( 'NONE', #19347, #11582, #319, .T. ) ;
#16811 = FACE_OUTER_BOUND ( 'NONE', #18597, .T. ) ;
#16812 = CONICAL_SURFACE ( 'NONE', #1364, 4.309401076758999416, 1.119376321708719590 ) ;
#16813 = ORIENTED_EDGE ( 'NONE', *, *, #9479, .T. ) ;
#16814 = CARTESIAN_POINT ( 'NONE',  ( -0.2682084311547999755, 25.15954001082000246, -2.144554451708999832 ) ) ;
#16815 = CARTESIAN_POINT ( 'NONE',  ( 6.470427684094998355, 13.53774001610998745, 1.516859935180999930 ) ) ;
#16816 = CARTESIAN_POINT ( 'NONE',  ( -1.780325977227999790, 27.77549822781000088, 1.403495832404999977 ) ) ;
#16817 = CARTESIAN_POINT ( 'NONE',  ( 0.000000000000000000, 20.00000000000000000, 0.000000000000000000 ) ) ;
#16818 = CARTESIAN_POINT ( 'NONE',  ( 18.85240113949000218, -1.886779804701000041, 10.26112574610000117 ) ) ;
#16819 = CARTESIAN_POINT ( 'NONE',  ( 23.99062354302999722, -13.93375672974000068, -0.8660254037843999608 ) ) ;
#16820 = DIRECTION ( 'NONE',  ( 1.000000000000000000, 0.000000000000000000, 0.000000000000000000 ) ) ;
#16821 =( NAMED_UNIT ( * ) SI_UNIT ( $, .STERADIAN. ) SOLID_ANGLE_UNIT ( ) );
#16822 = CARTESIAN_POINT ( 'NONE',  ( -13.15804650426999878, -7.258886979407000339, -7.170289537978000283 ) ) ;
#16823 = AXIS2_PLACEMENT_3D ( 'NONE', #11399, #22172, #15012 ) ;
#16824 = LINE ( 'NONE', #12846, #12111 ) ;
#16825 = CARTESIAN_POINT ( 'NONE',  ( -14.41332695378558171, 3.614289100492464435, 12.49991738134775865 ) ) ;
#16826 = EDGE_LOOP ( 'NONE', ( #2660, #13703, #15581, #15022 ) ) ;
#16827 = CARTESIAN_POINT ( 'NONE',  ( -10.26401792859842388, 15.76285626141247320, -1.163543192562826123 ) ) ;
#16828 = CARTESIAN_POINT ( 'NONE',  ( 0.2699447682128000015, 24.59981568338000102, 2.319434643344000069 ) ) ;
#16829 = CARTESIAN_POINT ( 'NONE',  ( 14.19210620200586526, -8.290201769613112504, -6.132491119281651137 ) ) ;
#16830 =( REPRESENTATION_RELATIONSHIP ('NONE','NONE', #13682, #16160 ) REPRESENTATION_RELATIONSHIP_WITH_TRANSFORMATION ( #3588 )SHAPE_REPRESENTATION_RELATIONSHIP( ) );
#16831 = DIRECTION ( 'NONE',  ( 0.000000000000000000, -1.000000000000000000, 0.000000000000000000 ) ) ;
#16832 = CARTESIAN_POINT ( 'NONE',  ( 21.84947845760000007, 5.758980354816999991, -9.655132153217000024 ) ) ;
#16833 = CARTESIAN_POINT ( 'NONE',  ( -1.973994283211000011, 29.25896236979000165, 1.294426475701000001 ) ) ;
#16834 = CARTESIAN_POINT ( 'NONE',  ( 14.00631938592161596, 6.815600421199946801, 5.980478541323148711 ) ) ;
#16835 = DIRECTION ( 'NONE',  ( -1.000000000000000000, 0.000000000000000000, 0.000000000000000000 ) ) ;
#16836 = CARTESIAN_POINT ( 'NONE',  ( -2.500000000000000000, 26.63419673618999894, 0.000000000000000000 ) ) ;
#16837 = CARTESIAN_POINT ( 'NONE',  ( -6.611979220525382672, 15.39629419157375700, 1.595713814164479771 ) ) ;
#16838 = CIRCLE ( 'NONE', #13355, 10.00000000000000000 ) ;
#16839 = CARTESIAN_POINT ( 'NONE',  ( 22.65115926907999722, -6.384260084937999125, 9.518811574639000739 ) ) ;
#16840 = ORIENTED_EDGE ( 'NONE', *, *, #8066, .T. ) ;
#16841 = AXIS2_PLACEMENT_3D ( 'NONE', #12601, #8968, #1093 ) ;
#16842 = DIRECTION ( 'NONE',  ( 0.000000000000000000, -1.000000000000000000, 0.000000000000000000 ) ) ;
#16843 = ORIENTED_EDGE ( 'NONE', *, *, #15881, .T. ) ;
#16844 = CARTESIAN_POINT ( 'NONE',  ( -16.22099577250664382, -4.576542577818303315, -7.940621211161685622 ) ) ;
#16845 = LINE ( 'NONE', #18673, #6162 ) ;
#16846 = CARTESIAN_POINT ( 'NONE',  ( 1.245756108708024223, 24.65778661989681098, 1.870434635796481393 ) ) ;
#16847 = CARTESIAN_POINT ( 'NONE',  ( 19.28334733059999806, -5.605041994797999472, 8.812776241869000771 ) ) ;
#16848 = CARTESIAN_POINT ( 'NONE',  ( -23.74465998031000069, -7.716878364870000340, 11.63397459621999985 ) ) ;
#16849 = PRODUCT_RELATED_PRODUCT_CATEGORY ( 'part', '', ( #22926 ) ) ;
#16850 = CARTESIAN_POINT ( 'NONE',  ( 2.157402177123000087, 25.41962896667000038, 1.099251314038999894 ) ) ;
#16851 = ORIENTED_EDGE ( 'NONE', *, *, #12648, .F. ) ;
#16852 = ORIENTED_EDGE ( 'NONE', *, *, #9193, .T. ) ;
#16853 = CARTESIAN_POINT ( 'NONE',  ( -1.536366799937290084, 27.31753006952332896, -1.999167105995447669 ) ) ;
#16854 = CARTESIAN_POINT ( 'NONE',  ( 0.000000000000000000, 24.50000000000000000, -4.618802153517000519 ) ) ;
#16855 = CARTESIAN_POINT ( 'NONE',  ( -24.50000000000292033, -10.56908696369845480, -6.693804389271431177 ) ) ;
#16856 = ORIENTED_EDGE ( 'NONE', *, *, #21675, .T. ) ;
#16857 = CARTESIAN_POINT ( 'NONE',  ( -24.50000000000000000, 10.82531754731000007, 6.250000000000000000 ) ) ;
#16858 = CARTESIAN_POINT ( 'NONE',  ( 19.14665134072065200, -9.780573450044347084, 3.801355032053034044 ) ) ;
#16859 = CONICAL_SURFACE ( 'NONE', #22643, 2.249999993254999886, 0.7853981633972997312 ) ;
#16860 = CARTESIAN_POINT ( 'NONE',  ( 12.50000000000000000, -13.93375672974000068, 0.1442505881487999853 ) ) ;
#16861 = CARTESIAN_POINT ( 'NONE',  ( 15.88567173426467782, -10.12137449307697246, -2.193410681915878069 ) ) ;
#16862 = CARTESIAN_POINT ( 'NONE',  ( -15.16085120776000039, 1.689811185772999824, -10.89268608759000045 ) ) ;
#16863 = CARTESIAN_POINT ( 'NONE',  ( -1.818533399173999809, 29.50782023400000043, 1.217198483556999999 ) ) ;
#16864 = CARTESIAN_POINT ( 'NONE',  ( -17.05828119693000033, -8.427367219174998425, -6.829844779585000580 ) ) ;
#16865 = CARTESIAN_POINT ( 'NONE',  ( 1.865992796466994230, 29.73627313755168089, 1.093859238132237843 ) ) ;
#16866 = ORIENTED_EDGE ( 'NONE', *, *, #6395, .T. ) ;
#16867 = CARTESIAN_POINT ( 'NONE',  ( -1.361207393629999984, 23.69359890096000143, -1.897971811607999992 ) ) ;
#16868 = CARTESIAN_POINT ( 'NONE',  ( -24.50000000000000000, -7.041797653771503462, -7.920532110923238278 ) ) ;
#16869 = CARTESIAN_POINT ( 'NONE',  ( -4.749999920006001020, 24.30000007999099765, -4.227385599170000255E-08 ) ) ;
#16870 = ORIENTED_EDGE ( 'NONE', *, *, #16310, .F. ) ;
#16871 = DIRECTION ( 'NONE',  ( 0.000000000000000000, 1.000000000000000000, 0.000000000000000000 ) ) ;
#16872 = CONICAL_SURFACE ( 'NONE', #619, 1.449999902385000095, 0.7853981633972997312 ) ;
#16873 = DIRECTION ( 'NONE',  ( 0.000000000000000000, 0.000000000000000000, -1.000000000000000000 ) ) ;
#16874 = ADVANCED_FACE ( 'NONE', ( #6256, #4327 ), #19093, .F. ) ;
#16875 = CARTESIAN_POINT ( 'NONE',  ( 13.58606375731000071, 0.1873974521201000054, -9.128548663592997769 ) ) ;
#16876 = ORIENTED_EDGE ( 'NONE', *, *, #23708, .T. ) ;
#16877 = CARTESIAN_POINT ( 'NONE',  ( -4.526039284669313822, 15.50981481425817421, 4.129000272277018269 ) ) ;
#16878 = CARTESIAN_POINT ( 'NONE',  ( 24.36414987671881960, -12.39811243366166416, 3.525839346946420427 ) ) ;
#16879 = ORIENTED_EDGE ( 'NONE', *, *, #16140, .F. ) ;
#16880 = CARTESIAN_POINT ( 'NONE',  ( -14.25699038479000080, 13.93375672974000068, 0.000000000000000000 ) ) ;
#16881 = CIRCLE ( 'NONE', #14190, 12.50000000000000178 ) ;
#16882 = CARTESIAN_POINT ( 'NONE',  ( -3.099999776787000005, 15.00000022320933013, -5.570936493763999179E-07 ) ) ;
#16883 = CARTESIAN_POINT ( 'NONE',  ( -3.633248405346000354, 12.23316262990001491, 3.176949996004001964 ) ) ;
#16884 = VECTOR ( 'NONE', #2405, 1000.000000000000000 ) ;
#16885 = CARTESIAN_POINT ( 'NONE',  ( -20.69122654991999966, 0.9355733309527999308, 9.531175163259002048 ) ) ;
#16886 = ADVANCED_FACE ( 'NONE', ( #13639, #20558 ), #3972, .T. ) ;
#16887 = CARTESIAN_POINT ( 'NONE',  ( 13.50000000000000000, 10.65000000000000036, 0.000000000000000000 ) ) ;
#16888 = DIRECTION ( 'NONE',  ( 0.9063077870366408328, 0.000000000000000000, -0.4226182617407188702 ) ) ;
#16889 = B_SPLINE_CURVE_WITH_KNOTS ( 'NONE', 3,
 ( #19042, #2452, #6809, #23391 ),
 .UNSPECIFIED., .F., .F.,
 ( 4, 4 ),
 ( 0.000000000000000000, 1.000000000000000000 ),
 .UNSPECIFIED. ) ;
#16890 = DIRECTION ( 'NONE',  ( -0.5000000000000169864, 0.000000000000000000, 0.8660254037844289376 ) ) ;
#16891 = CONICAL_SURFACE ( 'NONE', #7996, 4.649999883068000273, 0.7853981633972997312 ) ;
#16892 = PRESENTATION_STYLE_ASSIGNMENT (( #418 ) ) ;
#16893 = DIRECTION ( 'NONE',  ( 0.000000000000000000, 1.000000000000000000, 0.000000000000000000 ) ) ;
#16894 = CARTESIAN_POINT ( 'NONE',  ( -0.6792780159082327796, 30.36314944672238170, 2.050295082915816192 ) ) ;
#16895 = ORIENTED_EDGE ( 'NONE', *, *, #6829, .T. ) ;
#16896 = CARTESIAN_POINT ( 'NONE',  ( 23.89879234312000023, -3.396759081369000288, 9.855968912026000339 ) ) ;
#16897 = LINE ( 'NONE', #7222, #1153 ) ;
#16898 = CARTESIAN_POINT ( 'NONE',  ( -23.56048242866723541, -7.487011069796704277, -5.627623744119698124 ) ) ;
#16899 = CARTESIAN_POINT ( 'NONE',  ( -22.19730416677924012, 7.811814599075145082, -7.288801720585950328 ) ) ;
#16900 = CARTESIAN_POINT ( 'NONE',  ( 0.04500887484489999452, 26.99114211382000050, 2.291988582794999729 ) ) ;
#16901 = VECTOR ( 'NONE', #19493, 1000.000000000000000 ) ;
#16902 = CARTESIAN_POINT ( 'NONE',  ( 23.99062354302999722, -6.216878364870000340, -12.50000000000000000 ) ) ;
#16903 = ORIENTED_EDGE ( 'NONE', *, *, #21197, .T. ) ;
#16904 = EDGE_CURVE ( 'NONE', #10277, #17895, #7038, .T. ) ;
#16905 = CARTESIAN_POINT ( 'NONE',  ( -18.66125422242449616, 5.045625058748018255, -9.162508174574998776 ) ) ;
#16906 = CARTESIAN_POINT ( 'NONE',  ( 24.36881528991173340, 12.37037615450637240, 3.573879991655171562 ) ) ;
#16907 = CIRCLE ( 'NONE', #23095, 14.43375672974000778 ) ;
#16908 = CARTESIAN_POINT ( 'NONE',  ( 0.000000000000000000, 15.00000000000000000, 0.000000000000000000 ) ) ;
#16909 = B_SPLINE_CURVE_WITH_KNOTS ( 'NONE', 3,
 ( #22206, #5394, #16396, #18345 ),
 .UNSPECIFIED., .F., .F.,
 ( 4, 4 ),
 ( 0.000000000000000000, 1.000000000000000000 ),
 .UNSPECIFIED. ) ;
#16910 = ORIENTED_EDGE ( 'NONE', *, *, #17195, .F. ) ;
#16911 = AXIS2_PLACEMENT_3D ( 'NONE', #6735, #3126, #8568 ) ;
#16912 = DIRECTION ( 'NONE',  ( 1.000000000000000000, 0.000000000000000000, 0.000000000000000000 ) ) ;
#16913 = CARTESIAN_POINT ( 'NONE',  ( 11.56500142131000075, -9.431037050546001055, -0.2079650321152999859 ) ) ;
#16914 = EDGE_CURVE ( 'NONE', #3216, #14758, #330, .T. ) ;
#16915 = CARTESIAN_POINT ( 'NONE',  ( 0.000000000000000000, 18.00000000000000000, 0.000000000000000000 ) ) ;
#16916 = CARTESIAN_POINT ( 'NONE',  ( -4.649999999999999467, 20.00000000000000000, 0.000000000000000000 ) ) ;
#16917 = CARTESIAN_POINT ( 'NONE',  ( 12.82233580085999947, 8.050892032625998951, -7.895715898540999866 ) ) ;
#16918 = CARTESIAN_POINT ( 'NONE',  ( -12.25000000000000000, 6.489681479813073750, -13.21205004727046095 ) ) ;
#16919 = AXIS2_PLACEMENT_3D ( 'NONE', #4721, #19372, #4470 ) ;
#16920 =( GEOMETRIC_REPRESENTATION_CONTEXT ( 3 ) GLOBAL_UNCERTAINTY_ASSIGNED_CONTEXT ( ( #7238 ) ) GLOBAL_UNIT_ASSIGNED_CONTEXT ( ( #12292, #6828, #21618 ) ) REPRESENTATION_CONTEXT ( 'NONE', 'WORKASPACE' ) );
#16921 = PLANE ( 'NONE',  #11049 ) ;
#16922 = CARTESIAN_POINT ( 'NONE',  ( 25.03442155319000051, -3.648015224982000149, 9.208730145795000155 ) ) ;
#16923 = PRODUCT_DEFINITION_SHAPE ( 'NONE', 'NONE',  #8728 ) ;
#16924 = CARTESIAN_POINT ( 'NONE',  ( 3.268181200173220002, 29.87490599056235041, 2.731916857836431234 ) ) ;
#16925 = ORIENTED_EDGE ( 'NONE', *, *, #2779, .F. ) ;
#16926 = CARTESIAN_POINT ( 'NONE',  ( 11.75290414220000024, 1.735136046860999981, -9.156654427831000476 ) ) ;
#16927 = CARTESIAN_POINT ( 'NONE',  ( 24.50000000000000355, 2.870590891033125036, 9.920898659907861017 ) ) ;
#16928 = CARTESIAN_POINT ( 'NONE',  ( -4.424063187269999808, 12.34346680701001375, 1.825612035066000560 ) ) ;
#16929 = EDGE_CURVE ( 'NONE', #479, #1813, #3863, .T. ) ;
#16930 = FACE_OUTER_BOUND ( 'NONE', #9112, .T. ) ;
#16931 = CARTESIAN_POINT ( 'NONE',  ( -22.29029390899000163, 6.203558690370000406, -9.220249974902001711 ) ) ;
#16932 = ORIENTED_EDGE ( 'NONE', *, *, #4833, .F. ) ;
#16933 = CARTESIAN_POINT ( 'NONE',  ( 0.000000000000000000, 7.049999902385000183, 0.000000000000000000 ) ) ;
#16934 = EDGE_LOOP ( 'NONE', ( #17863, #13036, #15408, #6207, #1382, #216 ) ) ;
#16935 = CARTESIAN_POINT ( 'NONE',  ( -24.48376588671094467, 1.022231981141815904, -12.50007328824528408 ) ) ;
#16936 = EDGE_CURVE ( 'NONE', #5409, #20267, #14271, .T. ) ;
#16937 = CARTESIAN_POINT ( 'NONE',  ( -2.500000000000000000, 28.00000000000000000, 0.000000000000000000 ) ) ;
#16938 = DIRECTION ( 'NONE',  ( 0.000000000000000000, 1.000000000000000000, 0.000000000000000000 ) ) ;
#16939 = CARTESIAN_POINT ( 'NONE',  ( 15.93808103379664942, 9.080284284670666395, 1.188479485729086127 ) ) ;
#16940 = ADVANCED_FACE ( 'NONE', ( #12451 ), #7819, .F. ) ;
#16941 = AXIS2_PLACEMENT_3D ( 'NONE', #5566, #18989, #9201 ) ;
#16942 = CARTESIAN_POINT ( 'NONE',  ( -12.24999999999999822, 13.59206128970241778, -6.344557540553090291 ) ) ;
#16943 = DIRECTION ( 'NONE',  ( -1.000000000000000000, 0.000000000000000000, 0.000000000000000000 ) ) ;
#16944 = B_SPLINE_CURVE_WITH_KNOTS ( 'NONE', 3,
 ( #13459, #22546, #16983, #9952, #20863, #743, #5841, #7782, #8146, #5725, #18921, #19033, #16855, #11778 ),
 .UNSPECIFIED., .F., .F.,
 ( 4, 2, 2, 2, 2, 2, 4 ),
 ( 0.000000000000000000, 0.2500000000000001665, 0.3750000000000001665, 0.5000000000000002220, 0.6250000000000002220, 0.7500000000000001110, 1.000000000000000000 ),
 .UNSPECIFIED. ) ;
#16945 = CARTESIAN_POINT ( 'NONE',  ( -12.95491615630000126, -0.8957832334074999903, -10.15856198502000041 ) ) ;
#16946 = CARTESIAN_POINT ( 'NONE',  ( 4.000000000000000000, 29.99040384242091051, 0.4670641126941218468 ) ) ;
#16947 = DIRECTION ( 'NONE',  ( 0.000000000000000000, 1.000000000000000000, 0.000000000000000000 ) ) ;
#16948 = VECTOR ( 'NONE', #23336, 1000.000000000000000 ) ;
#16949 = ORIENTED_EDGE ( 'NONE', *, *, #11697, .T. ) ;
#16950 = EDGE_CURVE ( 'NONE', #20095, #6198, #9256, .T. ) ;
#16951 = CARTESIAN_POINT ( 'NONE',  ( -3.999999999999999112, 29.91068681084913905, 1.228746328088897721 ) ) ;
#16952 = ADVANCED_FACE ( 'NONE', ( #10517 ), #21405, .T. ) ;
#16953 = CARTESIAN_POINT ( 'NONE',  ( 2.275265428382999833, 24.62246328160999909, 1.096212662431000018 ) ) ;
#16954 = AXIS2_PLACEMENT_3D ( 'NONE', #21541, #4956, #19483 ) ;
#16955 = CARTESIAN_POINT ( 'NONE',  ( 14.19115849146925434, -8.310449043169278127, -6.104973310725267055 ) ) ;
#16956 = AXIS2_PLACEMENT_3D ( 'NONE', #21788, #5203, #525 ) ;
#16957 = LINE ( 'NONE', #3770, #15259 ) ;
#16958 = CARTESIAN_POINT ( 'NONE',  ( 22.58366630947000075, 0.6838113323537999833, 11.24159121164000119 ) ) ;
#16959 = CARTESIAN_POINT ( 'NONE',  ( 1.797218016695999898, 28.57905665442000043, 1.813427700862999981 ) ) ;
#16960 = CARTESIAN_POINT ( 'NONE',  ( 11.59051697470635922, -3.660525265868878275, 12.49991113089975947 ) ) ;
#16961 = CARTESIAN_POINT ( 'NONE',  ( 18.62948117788694802, 5.836193035541882068, 8.699610836940262715 ) ) ;
#16962 = CIRCLE ( 'NONE', #9245, 9.974367097859005327 ) ;
#16963 = CARTESIAN_POINT ( 'NONE',  ( -2.500000000000000000, 29.83419673618999823, 0.000000000000000000 ) ) ;
#16964 = CARTESIAN_POINT ( 'NONE',  ( 24.15736593521747011, -13.39690473052857378, -1.795880342563474397 ) ) ;
#16965 = ORIENTED_EDGE ( 'NONE', *, *, #14566, .T. ) ;
#16966 = CARTESIAN_POINT ( 'NONE',  ( -19.24432910583999856, 9.165129126472001175, 0.000000000000000000 ) ) ;
#16967 = ORIENTED_EDGE ( 'NONE', *, *, #7310, .T. ) ;
#16968 = AXIS2_PLACEMENT_3D ( 'NONE', #20843, #2072, #11287 ) ;
#16969 = CARTESIAN_POINT ( 'NONE',  ( 18.62128936713000371, -9.149140698829999252, 0.000000000000000000 ) ) ;
#16970 = CARTESIAN_POINT ( 'NONE',  ( -11.00000000000000000, 1.359357947053999856E-14, 0.000000000000000000 ) ) ;
#16971 = CARTESIAN_POINT ( 'NONE',  ( -21.96532910583999865, -9.234955349282000014, 0.000000000000000000 ) ) ;
#16972 = ORIENTED_EDGE ( 'NONE', *, *, #15743, .F. ) ;
#16973 = AXIS2_PLACEMENT_3D ( 'NONE', #13435, #22876, #19007 ) ;
#16974 = CARTESIAN_POINT ( 'NONE',  ( 16.79086406172000068, 10.59994276663999990, 3.220549048678999604 ) ) ;
#16975 = DIRECTION ( 'NONE',  ( 0.000000000000000000, -1.000000000000000000, 0.000000000000000000 ) ) ;
#16976 = CARTESIAN_POINT ( 'NONE',  ( -2.030073792688000367, 26.58962896666999853, -1.733846816783999989 ) ) ;
#16977 = EDGE_LOOP ( 'NONE', ( #10035, #10586, #5947, #23066, #16384 ) ) ;
#16978 = VERTEX_POINT ( 'NONE', #16056 ) ;
#16979 = CARTESIAN_POINT ( 'NONE',  ( -14.00000000000000178, -7.401164869303885396, -6.642430693032337352 ) ) ;
#16980 = CARTESIAN_POINT ( 'NONE',  ( -9.479727211694999767, 6.392817954487000520, -14.19584414485000146 ) ) ;
#16981 = AXIS2_PLACEMENT_3D ( 'NONE', #12834, #18185, #11136 ) ;
#16982 = DIRECTION ( 'NONE',  ( -1.000000000000000000, 0.000000000000000000, 0.000000000000000000 ) ) ;
#16983 = CARTESIAN_POINT ( 'NONE',  ( -23.97728971651672580, -8.249343195707872667, -10.71120260264468982 ) ) ;
#16984 = ORIENTED_EDGE ( 'NONE', *, *, #9965, .T. ) ;
#16985 = CARTESIAN_POINT ( 'NONE',  ( -20.80224598535999903, -1.543422969988999860, 9.524520383917000288 ) ) ;
#16986 = CARTESIAN_POINT ( 'NONE',  ( -14.40719396494353433, 12.69649082866680523, 3.008800086016248709 ) ) ;
#16987 = CARTESIAN_POINT ( 'NONE',  ( 19.05840758201121687, -8.181074449885935351, 6.563687483177104376 ) ) ;
#16988 = CARTESIAN_POINT ( 'NONE',  ( 6.205361592948507976, 13.85340785436878441, 0.9861407796932231129 ) ) ;
#16989 = CARTESIAN_POINT ( 'NONE',  ( 15.76648294310377807, -10.14853226314255608, 2.049597006397073429 ) ) ;
#16990 = CARTESIAN_POINT ( 'NONE',  ( -14.25753463260000053, -1.547198325978000000, 10.88880281900999947 ) ) ;
#16991 = CARTESIAN_POINT ( 'NONE',  ( 2.100031370072000136, 29.55149146746000000, 0.6307504428255000795 ) ) ;
#16992 = AXIS2_PLACEMENT_3D ( 'NONE', #14051, #4858, #19386 ) ;
#16993 = CARTESIAN_POINT ( 'NONE',  ( -12.54865546036000090, 9.084388929069001861, -2.336084003038000123 ) ) ;
#16994 = CARTESIAN_POINT ( 'NONE',  ( 1.013493880231960853, 29.66610983716606498, 1.907327710277805233 ) ) ;
#16995 = ORIENTED_EDGE ( 'NONE', *, *, #7908, .T. ) ;
#16996 = CARTESIAN_POINT ( 'NONE',  ( 2.179541537902999870, 25.03809824813999896, -0.09213785550823000436 ) ) ;
#16997 = CARTESIAN_POINT ( 'NONE',  ( 19.10756701789335210, -3.879051868053418950, 9.750401366061593578 ) ) ;
#16998 = CARTESIAN_POINT ( 'NONE',  ( -7.500000000000000000, 24.99999999999999645, -6.000000000000000000 ) ) ;
#16999 = ORIENTED_EDGE ( 'NONE', *, *, #6717, .T. ) ;
#17000 = CARTESIAN_POINT ( 'NONE',  ( 17.42999999999999972, 9.118569865760999704, 0.000000000000000000 ) ) ;
#17001 = CARTESIAN_POINT ( 'NONE',  ( -4.770941035428000632, 13.03080120692000143, 5.112121747560996354 ) ) ;
#17002 = DIRECTION ( 'NONE',  ( 0.000000000000000000, 0.000000000000000000, 1.000000000000000000 ) ) ;
#17003 = AXIS2_PLACEMENT_3D ( 'NONE', #6243, #20667, #13512 ) ;
#17004 = CARTESIAN_POINT ( 'NONE',  ( 17.23218892130999791, -6.764005061571999988, -7.001918906472000437 ) ) ;
#17005 = ORIENTED_EDGE ( 'NONE', *, *, #1552, .T. ) ;
#17006 = CARTESIAN_POINT ( 'NONE',  ( -6.132854427276997811, 15.85506591466998394, -1.061654000538000409 ) ) ;
#17007 = DIRECTION ( 'NONE',  ( 0.8660254037844288266, 0.5000000000000169864, 0.000000000000000000 ) ) ;
#17008 = ORIENTED_EDGE ( 'NONE', *, *, #7616, .T. ) ;
#17009 = DIRECTION ( 'NONE',  ( 1.000000000000000000, 0.000000000000000000, 0.000000000000000000 ) ) ;
#17010 = CARTESIAN_POINT ( 'NONE',  ( 21.24695833333333184, 7.370235643207817766, 5.663892701536951790 ) ) ;
#17011 = CARTESIAN_POINT ( 'NONE',  ( 2.811787122143001749, 11.98948095905999267, 3.831734478701003255 ) ) ;
#17012 = CARTESIAN_POINT ( 'NONE',  ( -10.04701370329000021, 16.31160201364000173, 0.9999999999983000265 ) ) ;
#17013 = CONICAL_SURFACE ( 'NONE', #7348, 14.24955550637000101, 0.7853981633972997312 ) ;
#17014 = CARTESIAN_POINT ( 'NONE',  ( 12.00000000000000178, -2.051339698423416458, -9.248432771917977746 ) ) ;
#17015 = CARTESIAN_POINT ( 'NONE',  ( 18.99920603379665351, -2.397423959588824705, -8.920410146158499032 ) ) ;
#17016 = CARTESIAN_POINT ( 'NONE',  ( -6.046837210729000489, 16.30334039894000142, -1.000000000000000000 ) ) ;
#17017 = DIRECTION ( 'NONE',  ( 1.000000000000000000, 0.000000000000000000, 0.000000000000000000 ) ) ;
#17018 = CARTESIAN_POINT ( 'NONE',  ( -2.500000000000000000, 29.03419673619000108, 0.000000000000000000 ) ) ;
#17019 = DIRECTION ( 'NONE',  ( 0.000000000000000000, -1.000000000000000000, 2.763497949612999920E-10 ) ) ;
#17020 = EDGE_CURVE ( 'NONE', #20353, #20749, #3323, .T. ) ;
#17021 = CARTESIAN_POINT ( 'NONE',  ( 2.157679587390584963, 30.59770904888307541, 0.1054980346066700797 ) ) ;
#17022 = EDGE_LOOP ( 'NONE', ( #911, #6725, #20465, #12755 ) ) ;
#17023 = CARTESIAN_POINT ( 'NONE',  ( 22.54603580819999920, -9.726366907112000249, -3.646778938341999954 ) ) ;
#17024 = CARTESIAN_POINT ( 'NONE',  ( 3.181525383082363323, 13.14482206580053081, -5.962137341915427768 ) ) ;
#17025 = B_SPLINE_CURVE_WITH_KNOTS ( 'NONE', 3,
 ( #326, #15096, #22492, #4094, #11490 ),
 .UNSPECIFIED., .F., .F.,
 ( 4, 1, 4 ),
 ( 0.000000000000000000, 0.3333333333333000081, 0.4999999999411116058 ),
 .UNSPECIFIED. ) ;
#17026 = CARTESIAN_POINT ( 'NONE',  ( -1.989999999999999991, 9.000000000000000000, 7.500000000000000000 ) ) ;
#17027 = CARTESIAN_POINT ( 'NONE',  ( -21.34046016612140662, -6.456723609324719781, 8.482265010774550973 ) ) ;
#17028 = CARTESIAN_POINT ( 'NONE',  ( 0.5061648749513000256, 28.64946440326000143, 2.249552142899000184 ) ) ;
#17029 = DIRECTION ( 'NONE',  ( -1.000000000000000000, 0.000000000000000000, 0.000000000000000000 ) ) ;
#17030 = ORIENTED_EDGE ( 'NONE', *, *, #15455, .T. ) ;
#17031 = CARTESIAN_POINT ( 'NONE',  ( -19.35893705290999733, -9.828989445528000246, 3.502754984265999738 ) ) ;
#17032 = EDGE_CURVE ( 'NONE', #21355, #20086, #7308, .T. ) ;
#17033 = CARTESIAN_POINT ( 'NONE',  ( 5.302302355349000074, 1.583778078195999810E-14, 0.000000000000000000 ) ) ;
#17034 = FACE_OUTER_BOUND ( 'NONE', #14618, .T. ) ;
#17035 = ORIENTED_EDGE ( 'NONE', *, *, #10608, .T. ) ;
#17036 = VERTEX_POINT ( 'NONE', #10867 ) ;
#17037 = LINE ( 'NONE', #16558, #20792 ) ;
#17038 = CARTESIAN_POINT ( 'NONE',  ( 18.16256424931000168, 7.359336859262000097, -7.874515470102998904 ) ) ;
#17039 = CARTESIAN_POINT ( 'NONE',  ( -18.00070722157999725, -1.604546417804000091, 11.29584027591999984 ) ) ;
#17040 = DIRECTION ( 'NONE',  ( 0.7071067811865462405, -0.7071067811865462405, 6.203608920934410591E-08 ) ) ;
#17041 = CARTESIAN_POINT ( 'NONE',  ( 12.68691913419000095, 3.375578516944000018, -10.11458711995999948 ) ) ;
#17042 = CARTESIAN_POINT ( 'NONE',  ( -12.30441696485953784, 6.530730161421050894, -13.29560061155498474 ) ) ;
#17043 = FACE_OUTER_BOUND ( 'NONE', #9174, .T. ) ;
#17044 = CARTESIAN_POINT ( 'NONE',  ( 25.18769339062000157, 0.3376592128354999889, 9.800598048666000039 ) ) ;
#17045 = ADVANCED_FACE ( 'NONE', ( #5291 ), #12797, .F. ) ;
#17046 = FACE_OUTER_BOUND ( 'NONE', #760, .T. ) ;
#17047 = ORIENTED_EDGE ( 'NONE', *, *, #21792, .T. ) ;
#17048 = CARTESIAN_POINT ( 'NONE',  ( 12.14717598830999989, 5.538504084190000398, -7.072432456372999887 ) ) ;
#17049 = CARTESIAN_POINT ( 'NONE',  ( 1.960438172910999866, 27.64956776952000084, -1.812210406530999851 ) ) ;
#17050 = AXIS2_PLACEMENT_3D ( 'NONE', #89, #20445, #16564 ) ;
#17051 = CARTESIAN_POINT ( 'NONE',  ( 4.915898507422000741, 12.43979313904999806, -0.02346798552494998302 ) ) ;
#17052 = CARTESIAN_POINT ( 'NONE',  ( 1.663296876077221098, 28.91427789370213475, 1.406703391654695601 ) ) ;
#17053 = CARTESIAN_POINT ( 'NONE',  ( -20.78653299696999923, -5.135752357527000100, -9.808972968573000273 ) ) ;
#17054 = ORIENTED_EDGE ( 'NONE', *, *, #6460, .F. ) ;
#17055 = LINE ( 'NONE', #4102, #6889 ) ;
#17056 = EDGE_LOOP ( 'NONE', ( #13350, #22457, #14813, #13944, #17154, #22850, #14705, #11681, #4292, #12577, #3412, #18449, #1604 ) ) ;
#17057 = CARTESIAN_POINT ( 'NONE',  ( -0.2163914088228000021, 23.55712358172999998, -2.044654028020000069 ) ) ;
#17058 = CARTESIAN_POINT ( 'NONE',  ( 6.696152422707000618, 29.50000000000000000, -6.000000000000000000 ) ) ;
#17060 = ADVANCED_FACE ( 'NONE', ( #12684 ), #3462, .T. ) ;
#17059 = CARTESIAN_POINT ( 'NONE',  ( -0.3106091461881000382, 27.87299822781000103, 2.245636445400999825 ) ) ;
#17061 = DIRECTION ( 'NONE',  ( 0.000000000000000000, 0.000000000000000000, -1.000000000000000000 ) ) ;
#17062 = CARTESIAN_POINT ( 'NONE',  ( 12.23943924931000105, -8.418214415862998123, -6.478404025908999664 ) ) ;
#17063 = CARTESIAN_POINT ( 'NONE',  ( -15.83949910911000281, -2.044365629921999883, 10.61848174243000109 ) ) ;
#17064 = CARTESIAN_POINT ( 'NONE',  ( 16.32825125730999716, -0.8629760640228999469, 9.162002845358001579 ) ) ;
#17065 = EDGE_CURVE ( 'NONE', #19197, #5360, #18361, .T. ) ;
#17066 = CARTESIAN_POINT ( 'NONE',  ( -14.40719416829650612, 3.742543968275074295, 12.49988362781941476 ) ) ;
#17067 = ORIENTED_EDGE ( 'NONE', *, *, #16113, .F. ) ;
#17068 = DIRECTION ( 'NONE',  ( 0.000000000000000000, 0.000000000000000000, -1.000000000000000000 ) ) ;
#17069 = CARTESIAN_POINT ( 'NONE',  ( 0.2919651418062000348, 24.49438105280999878, 2.508639337735000030 ) ) ;
#17070 = CARTESIAN_POINT ( 'NONE',  ( 13.76737141588828095, -6.929425286909939530, 7.636379834157821733 ) ) ;
#17071 = CARTESIAN_POINT ( 'NONE',  ( -6.000000000000000000, 26.50000000000000000, -6.000000000000000000 ) ) ;
#17072 = FACE_OUTER_BOUND ( 'NONE', #17114, .T. ) ;
#17073 = EDGE_CURVE ( 'NONE', #23198, #18177, #18020, .T. ) ;
#17074 = CARTESIAN_POINT ( 'NONE',  ( -0.3955362644989000587, 28.45937517842000020, 2.431766998741000219 ) ) ;
#17075 = CARTESIAN_POINT ( 'NONE',  ( 11.48696334737260649, -3.271224437879229008, 12.49992143329651384 ) ) ;
#17076 = EDGE_CURVE ( 'NONE', #15891, #9532, #9281, .T. ) ;
#17077 = CARTESIAN_POINT ( 'NONE',  ( 18.51797238626636499, 8.753726328939421819, 5.912621535854910348 ) ) ;
#17078 = DIRECTION ( 'NONE',  ( -1.000000000000000000, 0.000000000000000000, 0.000000000000000000 ) ) ;
#17079 = CARTESIAN_POINT ( 'NONE',  ( -6.081455072267000439, 16.30616274740000193, 0.9999994084348999834 ) ) ;
#17080 = B_SPLINE_CURVE_WITH_KNOTS ( 'NONE', 3,
 ( #9274, #20061, #20531, #13138, #54 ),
 .UNSPECIFIED., .F., .F.,
 ( 4, 1, 4 ),
 ( 0.000000000000000000, 0.5000000000000000000, 1.000000000000000000 ),
 .UNSPECIFIED. ) ;
#17081 = CARTESIAN_POINT ( 'NONE',  ( 0.000000000000000000, 18.50000000000000000, 0.000000000000000000 ) ) ;
#17082 = VERTEX_POINT ( 'NONE', #13019 ) ;
#17083 = CARTESIAN_POINT ( 'NONE',  ( 12.52688711657000020, -13.93375672974000068, 0.8660254037843999608 ) ) ;
#17084 = ORIENTED_EDGE ( 'NONE', *, *, #1692, .F. ) ;
#17085 = CARTESIAN_POINT ( 'NONE',  ( -1.463919501975000204, 24.98815194586000032, 2.312767826279999994 ) ) ;
#17086 = AXIS2_PLACEMENT_3D ( 'NONE', #15657, #773, #18947 ) ;
#17088 = CARTESIAN_POINT ( 'NONE',  ( 1.336097305351384046, 24.08750628805587368, 1.739191107916495227 ) ) ;
#17087 = CARTESIAN_POINT ( 'NONE',  ( 11.74999999482999868, 0.000000000000000000, 0.000000000000000000 ) ) ;
#17089 = ADVANCED_FACE ( 'NONE', ( #18143 ), #17592, .F. ) ;
#17090 = CARTESIAN_POINT ( 'NONE',  ( -12.24999999459000044, 1.554281285377000029E-14, 1.045589212608000028E-14 ) ) ;
#17091 = EDGE_LOOP ( 'NONE', ( #19516, #9345, #10662, #22045 ) ) ;
#17092 = CARTESIAN_POINT ( 'NONE',  ( 16.57658386292000330, 6.394698053106999680, -9.039278891232999769 ) ) ;
#17093 = CARTESIAN_POINT ( 'NONE',  ( -6.203295285168947792, 15.80526711864483858, 1.136188345634133512 ) ) ;
#17094 = CARTESIAN_POINT ( 'NONE',  ( -2.447990496630999768, 25.70419433610000226, -1.500144717171000064 ) ) ;
#17095 = ORIENTED_EDGE ( 'NONE', *, *, #751, .F. ) ;
#17096 = ORIENTED_EDGE ( 'NONE', *, *, #275, .T. ) ;
#17097 = CARTESIAN_POINT ( 'NONE',  ( -14.00000000000000355, -8.100261608394585977, -5.884167551250959249 ) ) ;
#17098 = VECTOR ( 'NONE', #19889, 1000.000000000000000 ) ;
#17099 = CARTESIAN_POINT ( 'NONE',  ( -11.21070971169000074, -8.063269234037999666, -13.31813143584999892 ) ) ;
#17100 = CARTESIAN_POINT ( 'NONE',  ( 1.738791845199069819, 6.997157444011510741, -0.2287927106351075324 ) ) ;
#17101 = CARTESIAN_POINT ( 'NONE',  ( 0.000000000000000000, 15.00000000000000000, 0.000000000000000000 ) ) ;
#17102 = ORIENTED_EDGE ( 'NONE', *, *, #11324, .T. ) ;
#17103 = CARTESIAN_POINT ( 'NONE',  ( -21.83044639899999950, -2.479786445640999482, -9.353611583463001367 ) ) ;
#17104 = DIRECTION ( 'NONE',  ( -1.000000000000000000, 0.000000000000000000, 0.000000000000000000 ) ) ;
#17105 = CARTESIAN_POINT ( 'NONE',  ( 6.200714323271902195, 13.87387049108663994, 0.9230690017325009489 ) ) ;
#17106 = CARTESIAN_POINT ( 'NONE',  ( 15.24483978148135854, 4.315420778289077219, 9.396116420522842461 ) ) ;
#17107 = DIRECTION ( 'NONE',  ( 0.000000000000000000, -1.000000000000000000, 0.000000000000000000 ) ) ;
#17108 = EDGE_CURVE ( 'NONE', #5087, #13716, #13146, .T. ) ;
#17109 = CARTESIAN_POINT ( 'NONE',  ( 2.133856304126000136, 29.00426108927999991, 0.4850359739721999963 ) ) ;
#17110 = ADVANCED_FACE ( 'NONE', ( #2009 ), #6146, .F. ) ;
#17111 = AXIS2_PLACEMENT_3D ( 'NONE', #19681, #12764, #5261 ) ;
#17112 = CARTESIAN_POINT ( 'NONE',  ( -13.80819562941000100, -8.705043851576000691, 6.319240472362000816 ) ) ;
#17113 = CARTESIAN_POINT ( 'NONE',  ( 1.254264882015703408, 29.68262165342926551, 1.758418893165299091 ) ) ;
#17114 = EDGE_LOOP ( 'NONE', ( #7856, #9690, #2311 ) ) ;
#17115 = CARTESIAN_POINT ( 'NONE',  ( -0.6595438615518000036, 25.38572581233000491, 2.254392134147999993 ) ) ;
#17116 = DIRECTION ( 'NONE',  ( 1.167437459203999868E-09, -4.746895044359150089E-20, 1.000000000000000000 ) ) ;
#17117 = ORIENTED_EDGE ( 'NONE', *, *, #10609, .T. ) ;
#17118 = CARTESIAN_POINT ( 'NONE',  ( -1.147416861493836482, 24.56833304100603854, -2.035450680677415303 ) ) ;
#17119 = DIRECTION ( 'NONE',  ( 1.000000000000000000, 0.000000000000000000, 0.000000000000000000 ) ) ;
#17120 = ADVANCED_FACE ( 'NONE', ( #9393 ), #9511, .F. ) ;
#17121 = EDGE_CURVE ( 'NONE', #2821, #19945, #19484, .T. ) ;
#17122 = CARTESIAN_POINT ( 'NONE',  ( 18.14804166666665708, -7.306463158791289381, 5.615200829187670273 ) ) ;
#17123 = CARTESIAN_POINT ( 'NONE',  ( 18.46518908530999781, 4.839936825908999651, 9.065913725881001639 ) ) ;
#17124 = EDGE_LOOP ( 'NONE', ( #16866, #13483, #14539, #21793 ) ) ;
#17125 = VECTOR ( 'NONE', #14316, 1000.000000000000000 ) ;
#17126 = CARTESIAN_POINT ( 'NONE',  ( -6.309791894495001330, 15.63766035666998455, -1.260321238843998604 ) ) ;
#17127 = CARTESIAN_POINT ( 'NONE',  ( 23.99062354302999722, 6.216878364870000340, 12.50000000000000000 ) ) ;
#17128 = PRODUCT ( 'Stem Lock Nut', 'Stem Lock Nut', '', ( #20293 ) ) ;
#17129 = ORIENTED_EDGE ( 'NONE', *, *, #1103, .T. ) ;
#17130 = DIRECTION ( 'NONE',  ( 0.000000000000000000, -1.000000000000000000, 0.000000000000000000 ) ) ;
#17131 = DIRECTION ( 'NONE',  ( -1.000000000000000000, 0.000000000000000000, 0.000000000000000000 ) ) ;
#17132 = CARTESIAN_POINT ( 'NONE',  ( 3.630035897976001902, 12.22073688872999853, 3.060979205723000085 ) ) ;
#17133 = CARTESIAN_POINT ( 'NONE',  ( -14.00000000000000000, -7.736145084527675131, 6.778938498890537900 ) ) ;
#17134 = CARTESIAN_POINT ( 'NONE',  ( -23.42120019438000256, -1.240814169192000049, -9.570677478896000068 ) ) ;
#17135 = CARTESIAN_POINT ( 'NONE',  ( -14.25243324638999809, 13.93375672974000068, 0.8660254037843999608 ) ) ;
#17136 = DIRECTION ( 'NONE',  ( 0.000000000000000000, 0.000000000000000000, 1.000000000000000000 ) ) ;
#17137 = DIRECTION ( 'NONE',  ( -0.000000000000000000, 1.000000000000000000, 0.000000000000000000 ) ) ;
#17138 = CARTESIAN_POINT ( 'NONE',  ( 5.243024108832019969, 13.88130074418577742, -4.105508865373297844 ) ) ;
#17139 = DIRECTION ( 'NONE',  ( 1.000000000000000000, 0.000000000000000000, 0.000000000000000000 ) ) ;
#17140 = CARTESIAN_POINT ( 'NONE',  ( 1.029509027115623088, 30.46714375698348221, 1.899064101531559912 ) ) ;
#17141 = VERTEX_POINT ( 'NONE', #13259 ) ;
#17142 = DIRECTION ( 'NONE',  ( 0.000000000000000000, 0.000000000000000000, -1.000000000000000000 ) ) ;
#17143 = CARTESIAN_POINT ( 'NONE',  ( 3.209708669317350438, 13.15082032542322032, -5.948897312515923019 ) ) ;
#17144 = PRODUCT_DEFINITION_FORMATION_WITH_SPECIFIED_SOURCE ( 'ANY', '', #22926, .NOT_KNOWN. ) ;
#17145 = FACE_OUTER_BOUND ( 'NONE', #2692, .T. ) ;
#17146 = CARTESIAN_POINT ( 'NONE',  ( -21.23335466603941768, -8.967721452004571603, 5.512103568260062758 ) ) ;
#17147 = CARTESIAN_POINT ( 'NONE',  ( -1.599833206071999969, 27.51196440325999859, -1.873164014766999896 ) ) ;
#17148 = AXIS2_PLACEMENT_3D ( 'NONE', #9597, #2206, #13582 ) ;
#17149 = CARTESIAN_POINT ( 'NONE',  ( 19.52828936713000019, 9.172416106433001204, 0.000000000000000000 ) ) ;
#17150 = ORIENTED_EDGE ( 'NONE', *, *, #18602, .T. ) ;
#17151 = CARTESIAN_POINT ( 'NONE',  ( -17.79600586831931253, -3.696083808623826794, 9.922044588331354831 ) ) ;
#17152 = CARTESIAN_POINT ( 'NONE',  ( -4.000000000000000000, 24.80000000000000426, -2.309401076759000304 ) ) ;
#17153 = CARTESIAN_POINT ( 'NONE',  ( 0.6140746919655077907, 27.86542664715151574, 2.111358184564343432 ) ) ;
#17154 = ORIENTED_EDGE ( 'NONE', *, *, #13547, .T. ) ;
#17155 = EDGE_CURVE ( 'NONE', #17699, #2459, #4155, .T. ) ;
#17156 = ORIENTED_EDGE ( 'NONE', *, *, #18997, .T. ) ;
#17157 = CARTESIAN_POINT ( 'NONE',  ( 4.000000000000000000, 29.69999999999999929, -2.309401076759000304 ) ) ;
#17158 = CARTESIAN_POINT ( 'NONE',  ( 12.21300158531000157, -1.561560366126000021, -9.991316461899998558 ) ) ;
#17159 = DIRECTION ( 'NONE',  ( -1.877655957117991099E-08, -0.9999999999999978906, 6.187284373139976848E-08 ) ) ;
#17160 = DIRECTION ( 'NONE',  ( 0.000000000000000000, -1.000000000000000000, 0.000000000000000000 ) ) ;
#17161 = CARTESIAN_POINT ( 'NONE',  ( 19.59411161192999984, -3.684212632671000520, 9.107267109273999850 ) ) ;
#17162 = CARTESIAN_POINT ( 'NONE',  ( -1.732016619652910761, 30.87844438891047005, -1.225611771103511494 ) ) ;
#17163 = DIRECTION ( 'NONE',  ( 1.000000000000000000, 0.000000000000000000, 0.000000000000000000 ) ) ;
#17164 = CARTESIAN_POINT ( 'NONE',  ( 21.46966224536999945, 3.294543478880000098, 9.128948853653000128 ) ) ;
#17165 = CARTESIAN_POINT ( 'NONE',  ( 15.90028936713000185, 9.079314476020000413, 0.000000000000000000 ) ) ;
#17166 = ORIENTED_EDGE ( 'NONE', *, *, #20638, .F. ) ;
#17167 = VECTOR ( 'NONE', #12503, 1000.000000000000000 ) ;
#17168 = DIRECTION ( 'NONE',  ( -1.127782589537999921E-10, -1.517608444995555245E-19, 1.000000000000000000 ) ) ;
#17169 = CARTESIAN_POINT ( 'NONE',  ( 1.887779699469000150, 27.45456776952000411, 1.887779699469000150 ) ) ;
#17170 = CARTESIAN_POINT ( 'NONE',  ( 3.263617933816000516, 12.03395420755000167, 3.428733546877001714 ) ) ;
#17171 = CARTESIAN_POINT ( 'NONE',  ( 2.154139288595608104, 29.01452026705025133, -0.1796810215235566943 ) ) ;
#17172 = CARTESIAN_POINT ( 'NONE',  ( -23.45988572945000072, 3.477105412697999665, 10.58835565412000079 ) ) ;
#17173 = ORIENTED_EDGE ( 'NONE', *, *, #19488, .T. ) ;
#17174 = CARTESIAN_POINT ( 'NONE',  ( -4.000000000000000000, 24.80000000000000426, -2.309401076759000304 ) ) ;
#17175 = ORIENTED_EDGE ( 'NONE', *, *, #15473, .F. ) ;
#17176 = CARTESIAN_POINT ( 'NONE',  ( 15.03108103379664939, -9.057008877067680430, -1.185432741998447614 ) ) ;
#17177 = CARTESIAN_POINT ( 'NONE',  ( -11.04281598264000053, 15.43375672938999976, 4.619452968294999437E-14 ) ) ;
#17178 = CARTESIAN_POINT ( 'NONE',  ( -7.034000000000000696, 1.310788454998999989E-14, 0.000000000000000000 ) ) ;
#17179 = CARTESIAN_POINT ( 'NONE',  ( -0.8309130272245487392, 6.827288109812859496, 1.546313273631122476 ) ) ;
#17180 = CARTESIAN_POINT ( 'NONE',  ( 16.18818924931000325, 2.089945795291999975, -10.52064088945999920 ) ) ;
#17181 = EDGE_CURVE ( 'NONE', #12251, #12959, #11457, .T. ) ;
#17182 = B_SPLINE_CURVE_WITH_KNOTS ( 'NONE', 3,
 ( #13648, #3866, #11256, #211 ),
 .UNSPECIFIED., .F., .F.,
 ( 4, 4 ),
 ( 0.000000000000000000, 1.000000000000000000 ),
 .UNSPECIFIED. ) ;
#17183 = AXIS2_PLACEMENT_3D ( 'NONE', #9977, #22684, #22803 ) ;
#17184 = CARTESIAN_POINT ( 'NONE',  ( -13.97056789615000127, 4.578996057282999743, 9.143398144881999201 ) ) ;
#17185 = CARTESIAN_POINT ( 'NONE',  ( 15.45075125730999943, 1.788522226178000052, -9.003565944673999510 ) ) ;
#17186 = CARTESIAN_POINT ( 'NONE',  ( 8.196152422706999729, 26.90192378864669820, 6.000000000000000000 ) ) ;
#17187 = ORIENTED_EDGE ( 'NONE', *, *, #7194, .F. ) ;
#17188 = CARTESIAN_POINT ( 'NONE',  ( 2.613167118632000019, 25.39225721452000073, -0.3773460266549999442 ) ) ;
#17189 = CARTESIAN_POINT ( 'NONE',  ( 13.84875374132612791, -8.743024429450152013, 5.452792944436931855 ) ) ;
#17190 = CONICAL_SURFACE ( 'NONE', #11013, 9.157130689899000586, 0.02565634000431304615 ) ;
#17191 = ORIENTED_EDGE ( 'NONE', *, *, #9059, .T. ) ;
#17192 = CARTESIAN_POINT ( 'NONE',  ( 3.874219016647000746, 14.52284758957000932, -4.808120738072998890 ) ) ;
#17193 = SURFACE_SIDE_STYLE ('',( #22520 ) ) ;
#17194 = CARTESIAN_POINT ( 'NONE',  ( 2.618739119015000227, 29.33532865103999754, 0.8251606127257998802 ) ) ;
#17195 = EDGE_CURVE ( 'NONE', #11527, #3987, #7330, .T. ) ;
#17196 = CARTESIAN_POINT ( 'NONE',  ( 14.40637819618423343, -4.518304899556225607, 7.830849211221313944 ) ) ;
#17197 = CARTESIAN_POINT ( 'NONE',  ( 17.96042842816580176, 2.416909556611977816, -10.17044595465547729 ) ) ;
#17198 = DIRECTION ( 'NONE',  ( 0.000000000000000000, 1.000000000000000000, 0.000000000000000000 ) ) ;
#17199 = DIRECTION ( 'NONE',  ( 0.000000000000000000, -1.000000000000000000, 0.000000000000000000 ) ) ;
#17200 = CARTESIAN_POINT ( 'NONE',  ( 24.43449445986660962, -11.92557563953692856, -4.344297082815015365 ) ) ;
#17201 = VERTEX_POINT ( 'NONE', #9870 ) ;
#17202 = FACE_OUTER_BOUND ( 'NONE', #7017, .T. ) ;
#17203 = VERTEX_POINT ( 'NONE', #416 ) ;
#17204 = DIRECTION ( 'NONE',  ( 0.000000000000000000, 0.000000000000000000, 1.000000000000000000 ) ) ;
#17206 = DIRECTION ( 'NONE',  ( 0.000000000000000000, 0.000000000000000000, -1.000000000000000000 ) ) ;
#17205 = CARTESIAN_POINT ( 'NONE',  ( -4.694832530803901172, 12.39124191863946045, 1.229044316482024835 ) ) ;
#17207 = CARTESIAN_POINT ( 'NONE',  ( -1.055729715565287385, 29.92936170367563520, -4.009276318043865750 ) ) ;
#17208 = VECTOR ( 'NONE', #22409, 1000.000000000000000 ) ;
#17209 = CARTESIAN_POINT ( 'NONE',  ( 16.39613296506999873, -0.1032919116580000157, -11.06709702821000008 ) ) ;
#17210 = CARTESIAN_POINT ( 'NONE',  ( 2.402140947178999647E-14, 29.00000000000000000, 2.500000000000000000 ) ) ;
#17211 = ADVANCED_FACE ( 'NONE', ( #7814, #22581 ), #4180, .F. ) ;
#17212 = CARTESIAN_POINT ( 'NONE',  ( 2.320116128650000054, 25.31419433610000169, 1.182158213329999930 ) ) ;
#17213 = VERTEX_POINT ( 'NONE', #532 ) ;
#17214 = ORIENTED_EDGE ( 'NONE', *, *, #23877, .T. ) ;
#17215 = CARTESIAN_POINT ( 'NONE',  ( -14.00000000000000178, 1.091918795757769178, -9.374698143281760210 ) ) ;
#17216 = DIRECTION ( 'NONE',  ( 0.000000000000000000, -1.000000000000000000, 0.000000000000000000 ) ) ;
#17217 = DIRECTION ( 'NONE',  ( 1.000000000000000000, 0.000000000000000000, 0.000000000000000000 ) ) ;
#17218 = EDGE_LOOP ( 'NONE', ( #12909, #2194, #7917 ) ) ;
#17219 = CARTESIAN_POINT ( 'NONE',  ( -21.90296809259000099, 3.348283013937999986, -9.636535320535001503 ) ) ;
#17220 = DIRECTION ( 'NONE',  ( -1.000000000000000000, 0.000000000000000000, 0.000000000000000000 ) ) ;
#17221 = CARTESIAN_POINT ( 'NONE',  ( 6.146734651151617435, 14.15406834883495790, 0.1968692019807686822 ) ) ;
#17222 = CARTESIAN_POINT ( 'NONE',  ( 15.70271885188221184, -9.447517964781408040, 4.243853946881596784 ) ) ;
#17223 = CARTESIAN_POINT ( 'NONE',  ( 2.205132044672000191, 30.37612098430000174, 0.8301523867869999851 ) ) ;
#17224 = ADVANCED_FACE ( 'NONE', ( #23054 ), #7846, .F. ) ;
#17225 = CARTESIAN_POINT ( 'NONE',  ( -20.51005101983020396, 9.225122117455688553, -5.023185617052088325 ) ) ;
#17226 = AXIS2_PLACEMENT_3D ( 'NONE', #16568, #13053, #14861 ) ;
#17227 = CARTESIAN_POINT ( 'NONE',  ( -18.68332398068000089, -2.538655790982999871, -10.59268337770999935 ) ) ;
#17228 = CARTESIAN_POINT ( 'NONE',  ( 0.4599695686195089950, 29.63102501646989850, 2.110344102147514445 ) ) ;
#17229 = ORIENTED_EDGE ( 'NONE', *, *, #9786, .T. ) ;
#17230 = CARTESIAN_POINT ( 'NONE',  ( -2.199644512527999751, 25.17633251583999865, -0.8239167990765999816 ) ) ;
#17231 = CARTESIAN_POINT ( 'NONE',  ( -5.372805085453999929, 16.07374366015000078, -2.940844016990000309 ) ) ;
#17232 = ORIENTED_EDGE ( 'NONE', *, *, #882, .T. ) ;
#17233 = CARTESIAN_POINT ( 'NONE',  ( -1.235289751754999887, 30.50000000000000000, -2.173490103315000255 ) ) ;
#17234 = CARTESIAN_POINT ( 'NONE',  ( -2.122520971047507921, 30.87747901625595759, 0.04286016723165855802 ) ) ;
#17235 = CARTESIAN_POINT ( 'NONE',  ( -20.25880420454665298, -7.349778174321106583, -5.648488567666000826 ) ) ;
#17236 = EDGE_CURVE ( 'NONE', #5281, #8904, #4611, .T. ) ;
#17237 = AXIS2_PLACEMENT_3D ( 'NONE', #147, #1745, #2093 ) ;
#17238 = CARTESIAN_POINT ( 'NONE',  ( 15.14812642130999976, -9.595485766438999420, 1.281252696419999948 ) ) ;
#17239 = ADVANCED_FACE ( 'NONE', ( #20711 ), #13797, .F. ) ;
#17240 = ORIENTED_EDGE ( 'NONE', *, *, #4312, .T. ) ;
#17241 = CIRCLE ( 'NONE', #23043, 1.899912543625999373 ) ;
#17242 = CARTESIAN_POINT ( 'NONE',  ( -6.042020549532005624, 15.62678062179001515, -1.260321238843998604 ) ) ;
#17243 = FACE_OUTER_BOUND ( 'NONE', #16744, .T. ) ;
#17244 = MANIFOLD_SOLID_BREP ( 'Stock-MAS-673-1', #21243 ) ;
#17245 = CARTESIAN_POINT ( 'NONE',  ( 0.000000000000000000, 21.50000000000000000, 0.000000000000000000 ) ) ;
#17246 = ORIENTED_EDGE ( 'NONE', *, *, #602, .F. ) ;
#17247 = B_SPLINE_CURVE_WITH_KNOTS ( 'NONE', 3,
 ( #9127, #142, #16501, #12765, #14690, #7071, #1511, #16383 ),
 .UNSPECIFIED., .F., .F.,
 ( 4, 2, 2, 4 ),
 ( 0.000000000000000000, 0.2499999999999998890, 0.4999999999999997780, 1.000000000000000000 ),
 .UNSPECIFIED. ) ;
#17248 = CARTESIAN_POINT ( 'NONE',  ( 4.000000000000000000, 26.39685207198629158, -1.322601766568779924 ) ) ;
#17249 = DIRECTION ( 'NONE',  ( 0.000000000000000000, -1.000000000000000000, 0.000000000000000000 ) ) ;
#17250 = CARTESIAN_POINT ( 'NONE',  ( 24.35303310461301152, -3.983639806630030034, 9.847948561538306222 ) ) ;
#17251 = DIRECTION ( 'NONE',  ( 0.000000000000000000, -1.000000000000000000, 0.000000000000000000 ) ) ;
#17252 = CARTESIAN_POINT ( 'NONE',  ( 18.37439921296329004, 8.632675712573684379, -5.842281130979909420 ) ) ;
#17253 = CARTESIAN_POINT ( 'NONE',  ( -5.833999999999999631, -1.199084044040999915E-14, 0.000000000000000000 ) ) ;
#17254 = CARTESIAN_POINT ( 'NONE',  ( -14.37382047448982014, 8.632461983038428599, -10.04764370666018714 ) ) ;
#17256 = ADVANCED_FACE ( 'NONE', ( #17072 ), #15809, .T. ) ;
#17255 = CARTESIAN_POINT ( 'NONE',  ( -4.008978351765000170, 13.27365510235000379, -4.673626722282001822 ) ) ;
#17257 = EDGE_CURVE ( 'NONE', #13296, #11734, #8126, .T. ) ;
#17258 = DIRECTION ( 'NONE',  ( 3.842525697690999187E-09, -0.9999999999999998890, -1.654014142263999949E-08 ) ) ;
#17259 = CARTESIAN_POINT ( 'NONE',  ( 1.999167105995449445, 28.71753006952332754, -1.536366799937288530 ) ) ;
#17260 = FACE_OUTER_BOUND ( 'NONE', #22079, .T. ) ;
#17261 = CARTESIAN_POINT ( 'NONE',  ( 2.103635563519576035, 30.57149230880223811, 0.5442943234456341095 ) ) ;
#17262 = ORIENTED_EDGE ( 'NONE', *, *, #5517, .T. ) ;
#17263 = CARTESIAN_POINT ( 'NONE',  ( 19.40145914081000100, 9.444312231696999405, -2.482237776557999709 ) ) ;
#17264 = CARTESIAN_POINT ( 'NONE',  ( -1.842050125101387659, 12.91841030608713048, -6.438214839482312435 ) ) ;
#17265 = AXIS2_PLACEMENT_3D ( 'NONE', #23008, #19019, #6425 ) ;
#17266 = CARTESIAN_POINT ( 'NONE',  ( -11.00000000000000000, 1.359357947053999856E-14, 0.000000000000000000 ) ) ;
#17267 = VECTOR ( 'NONE', #22694, 1000.000000000000000 ) ;
#17268 = CARTESIAN_POINT ( 'NONE',  ( -20.77815629069096559, -5.457173657242292641, -8.988420674274129496 ) ) ;
#17269 = CARTESIAN_POINT ( 'NONE',  ( 0.1450207862197000208, 27.41446440326000200, -2.459101194521000178 ) ) ;
#17270 = CARTESIAN_POINT ( 'NONE',  ( -3.653528746112522541, 24.70780860099737453, -2.509315635920815524 ) ) ;
#17271 = ORIENTED_EDGE ( 'NONE', *, *, #11060, .F. ) ;
#17272 = CARTESIAN_POINT ( 'NONE',  ( -17.46107102157156987, -10.41957730825670936, 0.5355958063994551432 ) ) ;
#17273 = DIRECTION ( 'NONE',  ( 0.000000000000000000, -1.000000000000000000, 0.000000000000000000 ) ) ;
#17274 = CIRCLE ( 'NONE', #10320, 2.899999999999999911 ) ;
#17275 = CARTESIAN_POINT ( 'NONE',  ( -0.7113715763943910808, 28.27224425180803280, -2.049892269754120200 ) ) ;
#17276 = CIRCLE ( 'NONE', #20004, 4.549999999999999822 ) ;
#17277 = ORIENTED_EDGE ( 'NONE', *, *, #12820, .T. ) ;
#17278 = ORIENTED_EDGE ( 'NONE', *, *, #3445, .F. ) ;
#17279 = CARTESIAN_POINT ( 'NONE',  ( 5.302302355349000074, 1.583778078195999810E-14, 0.000000000000000000 ) ) ;
#17280 = CARTESIAN_POINT ( 'NONE',  ( 16.84631424931000154, 6.637278256850999369, 8.448060240267999177 ) ) ;
#17281 = CARTESIAN_POINT ( 'NONE',  ( -14.20688765586999303, 1.535651113041606619, -8.952319352988645562 ) ) ;
#17282 = DIRECTION ( 'NONE',  ( -1.000000000000000000, 0.000000000000000000, 0.000000000000000000 ) ) ;
#17283 = CARTESIAN_POINT ( 'NONE',  ( 22.83420833333331501, 9.257252502730580090, -1.211898466613929637 ) ) ;
#17284 = CARTESIAN_POINT ( 'NONE',  ( 19.25556994526000310, 7.389816571954000324, 7.286178097052999902 ) ) ;
#17285 = DIRECTION ( 'NONE',  ( 1.000000000000000000, 0.000000000000000000, 0.000000000000000000 ) ) ;
#17286 = DIRECTION ( 'NONE',  ( 1.000000000000000000, -4.862256430815421556E-10, 0.000000000000000000 ) ) ;
#17287 = CARTESIAN_POINT ( 'NONE',  ( 23.59425147122999888, -6.506847782497000132, 7.278924568632000103 ) ) ;
#17288 = LINE ( 'NONE', #11846, #18931 ) ;
#17289 = ORIENTED_EDGE ( 'NONE', *, *, #20077, .T. ) ;
#17290 = DIRECTION ( 'NONE',  ( 0.000000000000000000, -1.000000000000000000, 0.000000000000000000 ) ) ;
#17291 = CARTESIAN_POINT ( 'NONE',  ( 0.5289967318967999654, 28.42163313894999987, -2.411020654974999733 ) ) ;
#17292 = CONICAL_SURFACE ( 'NONE', #2598, 4.699999872533999756, 0.7853981633972997312 ) ;
#17293 = CARTESIAN_POINT ( 'NONE',  ( 4.683509707950999079, 12.52043781250001153, 0.6549564855534005803 ) ) ;
#17294 = DIRECTION ( 'NONE',  ( 0.000000000000000000, 1.000000000000000000, 0.000000000000000000 ) ) ;
#17295 = CARTESIAN_POINT ( 'NONE',  ( -23.12571663788999743, -8.293331836127999068, 7.431160843878000577 ) ) ;
#17296 = EDGE_LOOP ( 'NONE', ( #16197, #14414, #771, #23658, #21722, #13052 ) ) ;
#17297 = VECTOR ( 'NONE', #22366, 1000.000000000000000 ) ;
#17298 = DIRECTION ( 'NONE',  ( 0.000000000000000000, -1.000000000000000000, 0.000000000000000000 ) ) ;
#17299 = EDGE_LOOP ( 'NONE', ( #16038, #4907, #5552, #21090 ) ) ;
#17300 = CARTESIAN_POINT ( 'NONE',  ( -24.41513307468559901, 2.047838742109346466, -12.49997210311845564 ) ) ;
#17301 = CARTESIAN_POINT ( 'NONE',  ( -1.600000000000000089, 8.900000000000000355, 1.856656273168999865E-09 ) ) ;
#17302 = CARTESIAN_POINT ( 'NONE',  ( 4.683882115557001846, 14.25929394625999080, 3.864918841593002696 ) ) ;
#17303 = CARTESIAN_POINT ( 'NONE',  ( 0.06268874648260357174, 6.777703239720367812, 1.750068228840472750 ) ) ;
#17304 = CARTESIAN_POINT ( 'NONE',  ( 12.05662674931000033, -10.44547366770999908, -0.2303471896619999904 ) ) ;
#17305 = CARTESIAN_POINT ( 'NONE',  ( -19.22500490859999900, -8.822855456895000614, 5.347747867906999630 ) ) ;
#17306 = CIRCLE ( 'NONE', #23104, 9.030549305585997999 ) ;
#17307 = CARTESIAN_POINT ( 'NONE',  ( 14.13450125731000107, 8.592455601080001060, 3.130286720869000394 ) ) ;
#17308 = CARTESIAN_POINT ( 'NONE',  ( -2.499999999999999556, 27.21666666666666146, 0.3272492347489423525 ) ) ;
#17309 = VERTEX_POINT ( 'NONE', #7992 ) ;
#17310 = CYLINDRICAL_SURFACE ( 'NONE', #19279, 10.59999999999999964 ) ;
#17311 = CARTESIAN_POINT ( 'NONE',  ( -2.231919210383000340, 23.57515785297000122, -0.1739934626373000059 ) ) ;
#17312 = CARTESIAN_POINT ( 'NONE',  ( 14.13913242659573299, -9.311690260717602641, -4.516683420423269979 ) ) ;
#17313 = ORIENTED_EDGE ( 'NONE', *, *, #1692, .T. ) ;
#17314 = CARTESIAN_POINT ( 'NONE',  ( -1.989847688386000124, 13.98044646450001061, -5.851777455581000709 ) ) ;
#17315 = CARTESIAN_POINT ( 'NONE',  ( -24.16119556692216364, 12.87912905767985450, -2.692171137914732171 ) ) ;
#17316 = CARTESIAN_POINT ( 'NONE',  ( -1.217060697036999928, 28.83266645185000243, -2.461188343967999792 ) ) ;
#17317 = CARTESIAN_POINT ( 'NONE',  ( 12.40357033524261254, -5.939957768490999435, 12.49999999999918820 ) ) ;
#17318 = CARTESIAN_POINT ( 'NONE',  ( 17.29137567844483669, -9.236652306994301398, 5.172519770036458908 ) ) ;
#17319 = CARTESIAN_POINT ( 'NONE',  ( -9.000000000000000000, 24.99999999999999645, -6.000000000000000000 ) ) ;
#17320 = DIRECTION ( 'NONE',  ( 0.000000000000000000, -1.000000000000000000, 0.000000000000000000 ) ) ;
#17321 = EDGE_CURVE ( 'NONE', #15235, #4168, #22013, .T. ) ;
#17322 = VERTEX_POINT ( 'NONE', #6175 ) ;
#17323 = CARTESIAN_POINT ( 'NONE',  ( 2.399426801160061462, 11.81735415996129568, -4.146195241240062224 ) ) ;
#17324 = VERTEX_POINT ( 'NONE', #10060 ) ;
#17325 = B_SPLINE_SURFACE_WITH_KNOTS ( 'NONE', 3, 3, ( 
 ( #603, #21209, #8375, #8004, #4624, #19395, #18907, #15379, #2808, #10190, #22533, #5939, #13325, #20724, #4130, #2315, #9703, #17085, #484, #7886, #6789, #1471, #14308, #16236, #4747, #4993, #10312, #6915, #8739, #21701, #4868, #12381, #14060, #3294, #1349 ),
 ( #19996, #3416, #8616, #12493, #16102, #2928, #12132, #7033, #1101, #8501, #23626, #10558, #21453, #21811, #6667, #5226, #3054, #21581, #3176, #12257, #23504, #10441, #19878, #5111, #10676, #12609, #19520, #10799, #15864, #18192, #17704, #1593, #23254, #17830, #1225 ),
 ( #15741, #14184, #14418, #23128, #6553, #13938, #15978, #19766, #21332, #23372, #7378, #106, #3751, #1935, #7615, #11022, #20343, #8250, #12946, #18644, #11140, #14760, #18526, #2050, #14650, #1817, #9323, #7493, #16697, #9203, #11383, #22158, #14878, #22264, #11267 ),
 ( #20232, #3874, #5569, #18754, #5803, #5681, #13067, #1698, #20466, #9441, #16814, #22390, #219, #14992, #20576, #18405, #13185, #3988, #8975, #16348, #23736, #14532, #21926, #16458, #22046, #5338, #12726, #20121, #3529, #18296, #9087, #23849, #5455, #7741, #17057 ) ),
 .UNSPECIFIED., .F., .F., .F.,
 ( 4, 4 ),
 ( 4, 1, 1, 1, 1, 1, 1, 1, 1, 1, 1, 1, 1, 1, 1, 1, 1, 1, 1, 1, 1, 1, 1, 1, 1, 1, 1, 1, 1, 1, 1, 1, 4 ),
 ( -0.3056682515952000023, 1.305668251594999996 ),
 ( -0.01429133938984000068, 0.008932087118648001159, 0.03215551362712999739, 0.05537894013562000284, 0.07860236664410000240, 0.1018257931525999999, 0.1250492196610999973, 0.1482726461695999809, 0.1714960726779999889, 0.1947194991865000002, 0.2179429256950000116, 0.2411663522034999951, 0.2643897787120000342, 0.2876132052204999900, 0.3108366317290000014, 0.3340600582373999816, 0.3572834847458999930, 0.3805069112544000043, 0.4037303377629000156, 0.4269537642714000270, 0.4501771907798999828, 0.4734006172883000185, 0.4966240437968000299, 0.5198474703052999857, 0.5430708968138000525, 0.5662943233223000083, 0.5895177498307999642, 0.6127411763393000310, 0.6359646028477000668, 0.6591880293561999116, 0.6824114558646999784, 0.7056348823732000453, 0.7288583088817000011 ),
 .UNSPECIFIED. ) ;
#17326 = DIRECTION ( 'NONE',  ( -1.000000000000000000, 0.000000000000000000, 0.000000000000000000 ) ) ;
#17328 = CARTESIAN_POINT ( 'NONE',  ( -2.061627795661847617, 24.55982949481376920, -0.7474695682632446214 ) ) ;
#17327 = CARTESIAN_POINT ( 'NONE',  ( -0.9971822219135534349, 11.51405072702774746, 4.736263398427000837 ) ) ;
#17329 = CARTESIAN_POINT ( 'NONE',  ( -4.000000000000000000, 26.20000000000000284, 2.309401076759000304 ) ) ;
#17330 = CARTESIAN_POINT ( 'NONE',  ( 14.95252578230999951, 10.54459643182000228, -3.229425179476999919 ) ) ;
#17331 = CARTESIAN_POINT ( 'NONE',  ( -20.78894092153334228, 5.513289374754998029, 7.448743673073256133 ) ) ;
#17332 = AXIS2_PLACEMENT_3D ( 'NONE', #2420, #9810, #7021 ) ;
#17333 = CARTESIAN_POINT ( 'NONE',  ( 2.108296854627000005, 27.06919433610000070, -1.948889566018999986 ) ) ;
#17334 = EDGE_CURVE ( 'NONE', #17770, #5775, #19435, .T. ) ;
#17335 = ORIENTED_EDGE ( 'NONE', *, *, #50, .T. ) ;
#17336 = EDGE_LOOP ( 'NONE', ( #20390, #269, #22739, #18353 ) ) ;
#17337 = CARTESIAN_POINT ( 'NONE',  ( -13.99999999999999822, 3.110363060826788484, -8.795536003872138409 ) ) ;
#17338 = AXIS2_PLACEMENT_3D ( 'NONE', #22687, #10107, #15786 ) ;
#17339 = CARTESIAN_POINT ( 'NONE',  ( -2.399999988616999591, 24.50000001138332806, -6.337991255853999810E-08 ) ) ;
#17340 = CARTESIAN_POINT ( 'NONE',  ( -14.33281118273068167, -8.249344442822355461, -10.71171629589809449 ) ) ;
#17341 = VERTEX_POINT ( 'NONE', #23241 ) ;
#17342 = FACE_OUTER_BOUND ( 'NONE', #18284, .T. ) ;
#17343 = DIRECTION ( 'NONE',  ( 1.000000000000000000, 0.000000000000000000, 0.000000000000000000 ) ) ;
#17344 = CARTESIAN_POINT ( 'NONE',  ( 15.88870756930322159, -10.09910537503753503, -2.295021277106512603 ) ) ;
#17345 = B_SPLINE_CURVE_WITH_KNOTS ( 'NONE', 3,
 ( #20146, #4014, #3553, #12977 ),
 .UNSPECIFIED., .F., .F.,
 ( 4, 4 ),
 ( 0.000000000000000000, 1.000000000000000000 ),
 .UNSPECIFIED. ) ;
#17346 = CONICAL_SURFACE ( 'NONE', #11215, 3.049999825846000157, 0.7853981633972997312 ) ;
#17347 = CARTESIAN_POINT ( 'NONE',  ( -16.03012606477000190, -7.866000996152999747, 7.756133801015000273 ) ) ;
#17348 = CARTESIAN_POINT ( 'NONE',  ( -8.099999999999999645, 1.323843189878000027E-14, 0.000000000000000000 ) ) ;
#17349 = CARTESIAN_POINT ( 'NONE',  ( -21.12769403777191357, -9.214013686813418147, -5.077623156764633272 ) ) ;
#17350 = CARTESIAN_POINT ( 'NONE',  ( 0.000000000000000000, 22.19999999999999574, -2.749999999999999556 ) ) ;
#17351 = ADVANCED_FACE ( 'NONE', ( #8360 ), #8892, .T. ) ;
#17352 = CARTESIAN_POINT ( 'NONE',  ( -0.9793716477997560510, 29.54380556444507633, 1.925535291027464346 ) ) ;
#17353 = ORIENTED_EDGE ( 'NONE', *, *, #11135, .F. ) ;
#17354 = CARTESIAN_POINT ( 'NONE',  ( -0.8474553701696999619, 24.26896156435000051, -2.190683491321000265 ) ) ;
#17355 = CIRCLE ( 'NONE', #9236, 2.100000000000000089 ) ;
#17356 = CARTESIAN_POINT ( 'NONE',  ( -16.95178362136691774, 7.756708774288529895, -7.108411929819117070 ) ) ;
#17357 = AXIS2_PLACEMENT_3D ( 'NONE', #9894, #11365, #7594 ) ;
#17358 = ORIENTED_EDGE ( 'NONE', *, *, #19654, .T. ) ;
#17359 = DIRECTION ( 'NONE',  ( 0.000000000000000000, 1.000000000000000000, 0.000000000000000000 ) ) ;
#17360 = CARTESIAN_POINT ( 'NONE',  ( 5.826396675508998868, 13.70895565241001179, -3.199610063967998741 ) ) ;
#17361 = CARTESIAN_POINT ( 'NONE',  ( -2.134263429621519048, 30.85404986398537019, 0.2236583631314258136 ) ) ;
#17362 = AXIS2_PLACEMENT_3D ( 'NONE', #15614, #11522, #22641 ) ;
#17363 = CARTESIAN_POINT ( 'NONE',  ( -24.50000000000000355, -0.1211919172565497221, -10.51440256396106854 ) ) ;
#17364 = EDGE_CURVE ( 'NONE', #8845, #17082, #16221, .T. ) ;
#17365 = CARTESIAN_POINT ( 'NONE',  ( 11.85750142130999940, -4.891210171397999851, -8.253706317253998392 ) ) ;
#17366 = ORIENTED_EDGE ( 'NONE', *, *, #4216, .T. ) ;
#17367 = CARTESIAN_POINT ( 'NONE',  ( 18.25370603379667145, -2.693211065087175893, 8.797714532981757429 ) ) ;
#17368 = PLANE ( 'NONE',  #1831 ) ;
#17369 = CARTESIAN_POINT ( 'NONE',  ( 24.07420734439604004, -13.66464621573615190, 1.332138486891153217 ) ) ;
#17370 = CIRCLE ( 'NONE', #12731, 13.93375672974000068 ) ;
#17371 = ORIENTED_EDGE ( 'NONE', *, *, #22099, .T. ) ;
#17372 = CARTESIAN_POINT ( 'NONE',  ( -2.090639349808711689, 24.68204389809848109, 0.7662985136386953888 ) ) ;
#17373 = CARTESIAN_POINT ( 'NONE',  ( 21.13358333333333050, 8.973854058736122852, 2.411525931920532440 ) ) ;
#17374 = CARTESIAN_POINT ( 'NONE',  ( 23.82357055235148380, 10.53309116123875633, 1.283855905984082835 ) ) ;
#17375 = CARTESIAN_POINT ( 'NONE',  ( -14.00000000000000000, -8.319952449050001420, 6.066771132503999020 ) ) ;
#17377 = CARTESIAN_POINT ( 'NONE',  ( 17.66135951571182616, -10.36152372384453280, -0.9047222416689953972 ) ) ;
#17376 = VECTOR ( 'NONE', #19477, 1000.000000000000114 ) ;
#17378 = AXIS2_PLACEMENT_3D ( 'NONE', #17692, #963, #1215 ) ;
#17379 = ADVANCED_FACE ( 'NONE', ( #3164 ), #10546, .T. ) ;
#17380 = DIRECTION ( 'NONE',  ( -1.000000000000000000, 0.000000000000000000, 0.000000000000000000 ) ) ;
#17381 = FACE_OUTER_BOUND ( 'NONE', #18782, .T. ) ;
#17382 = CARTESIAN_POINT ( 'NONE',  ( 21.73978222679999917, 10.36410918087999988, -4.347985533771000277 ) ) ;
#17383 = DIRECTION ( 'NONE',  ( 1.000000000000000000, 0.000000000000000000, 0.000000000000000000 ) ) ;
#17384 = CIRCLE ( 'NONE', #6949, 0.09999999999999939493 ) ;
#17385 = CARTESIAN_POINT ( 'NONE',  ( 0.3272492347489341924, 28.81753006952333251, -2.500000000000000888 ) ) ;
#17386 = CARTESIAN_POINT ( 'NONE',  ( 0.000000000000000000, 19.00000000000000000, 0.000000000000000000 ) ) ;
#17387 = ADVANCED_FACE ( 'NONE', ( #14170 ), #348, .T. ) ;
#17388 = CARTESIAN_POINT ( 'NONE',  ( -1.378834737919759856, 30.31601879608736638, 1.669154270543806051 ) ) ;
#17389 = ORIENTED_EDGE ( 'NONE', *, *, #21571, .T. ) ;
#17390 = EDGE_CURVE ( 'NONE', #11075, #23046, #13121, .T. ) ;
#17391 = CARTESIAN_POINT ( 'NONE',  ( 23.06000586213199455, 7.405742005601795519, 5.691048056048777504 ) ) ;
#17392 = CARTESIAN_POINT ( 'NONE',  ( 21.24584100372000250, -3.048715644316999818, -10.45155468166000112 ) ) ;
#17393 = CARTESIAN_POINT ( 'NONE',  ( -1.017692192065588586, 12.83700921921063909, -6.598984237050126822 ) ) ;
#17394 = CARTESIAN_POINT ( 'NONE',  ( 0.6950034797113092688, 29.87418302490042876, 4.217541707417931107 ) ) ;
#17395 = CIRCLE ( 'NONE', #6954, 2.949999999999999734 ) ;
#17396 = CARTESIAN_POINT ( 'NONE',  ( -20.18907604024003177, 10.46691963189587327, -0.7924825188483891614 ) ) ;
#17397 = FACE_OUTER_BOUND ( 'NONE', #12293, .T. ) ;
#17398 = CONICAL_SURFACE ( 'NONE', #3447, 2.249999993254999886, 0.7853981633972997312 ) ;
#17399 = B_SPLINE_CURVE_WITH_KNOTS ( 'NONE', 3,
 ( #761, #22916, #17610, #21241 ),
 .UNSPECIFIED., .F., .F.,
 ( 4, 4 ),
 ( 0.000000000000000000, 1.000000000000000000 ),
 .UNSPECIFIED. ) ;
#17400 = CARTESIAN_POINT ( 'NONE',  ( -1.670409819853669209, 27.99999999999984013, 3.654390594367815215 ) ) ;
#17401 = VERTEX_POINT ( 'NONE', #12598 ) ;
#17402 = CARTESIAN_POINT ( 'NONE',  ( -17.23778112373701887, -7.827069389925411791, -6.885115441211981491 ) ) ;
#17403 = EDGE_CURVE ( 'NONE', #1857, #23530, #9054, .T. ) ;
#17404 = DIRECTION ( 'NONE',  ( -0.7071067811867999264, 0.7071067811862000729, 3.665336534966999651E-07 ) ) ;
#17405 = CARTESIAN_POINT ( 'NONE',  ( -1.676242427568033211, 27.71749297273097312, 1.380892551129798251 ) ) ;
#17406 = DIRECTION ( 'NONE',  ( 0.000000000000000000, 0.000000000000000000, 1.000000000000000000 ) ) ;
#17407 = EDGE_LOOP ( 'NONE', ( #15513, #1987, #22481, #18894, #1309 ) ) ;
#17408 = ORIENTED_EDGE ( 'NONE', *, *, #7098, .F. ) ;
#17409 = CARTESIAN_POINT ( 'NONE',  ( 4.000000000000000888, 29.87490599056224383, -1.464369514602714251 ) ) ;
#17410 = CARTESIAN_POINT ( 'NONE',  ( 11.81081408531000143, -9.938255359128000066, -0.2191561108886999898 ) ) ;
#17411 = CARTESIAN_POINT ( 'NONE',  ( -24.54069805790000203, -5.308769442286998874, -9.260118962789000818 ) ) ;
#17412 = CARTESIAN_POINT ( 'NONE',  ( -16.30463496464999906, -10.28730417320999990, -0.2735448704119000096 ) ) ;
#17413 = CARTESIAN_POINT ( 'NONE',  ( 19.20620833333333621, 9.164150872317845753, -1.199711491691351162 ) ) ;
#17414 = CARTESIAN_POINT ( 'NONE',  ( 16.47999951746000136, -9.167179358941000444, 3.350482958538000045 ) ) ;
#17415 = CARTESIAN_POINT ( 'NONE',  ( -3.999999999999999112, 26.29977277844471573, -1.897803675662255385 ) ) ;
#17416 = CARTESIAN_POINT ( 'NONE',  ( 2.402140947178999647E-14, 29.00000000000000000, 2.500000000000000000 ) ) ;
#17417 = CARTESIAN_POINT ( 'NONE',  ( 19.60491575378000206, -4.129469127383999627, 9.308132072280001168 ) ) ;
#17418 = B_SPLINE_CURVE_WITH_KNOTS ( 'NONE', 3,
 ( #15937, #3008, #21295, #23332, #21408, #1184, #18023, #1307, #23456, #16184 ),
 .UNSPECIFIED., .F., .F.,
 ( 4, 1, 1, 2, 2, 4 ),
 ( 0.000000000000000000, 0.2500000000000001665, 0.3750000000000001665, 0.4375000000000000555, 0.4999999999999999445, 1.000000000000000000 ),
 .UNSPECIFIED. ) ;
#17419 = DIRECTION ( 'NONE',  ( 0.000000000000000000, 1.000000000000000000, 0.000000000000000000 ) ) ;
#17420 = ORIENTED_EDGE ( 'NONE', *, *, #18394, .F. ) ;
#17421 = CARTESIAN_POINT ( 'NONE',  ( 0.000000000000000000, 28.30000000000000071, 4.618802153517000519 ) ) ;
#17422 = CARTESIAN_POINT ( 'NONE',  ( 1.016344414748000080, 28.90913313895000059, 1.994688225595000253 ) ) ;
#17423 = CARTESIAN_POINT ( 'NONE',  ( 4.661177797444999271, 12.43313903173000234, 1.085618546728999378 ) ) ;
#17424 = CARTESIAN_POINT ( 'NONE',  ( 2.059625858907598417, 28.96477123800895725, 0.6504964593587068133 ) ) ;
#17425 = CARTESIAN_POINT ( 'NONE',  ( -19.28277208493999950, -10.43152901666999810, -0.1440240251737999744 ) ) ;
#17426 = DIRECTION ( 'NONE',  ( -1.000000000000000000, 0.000000000000000000, 0.000000000000000000 ) ) ;
#17427 = ORIENTED_EDGE ( 'NONE', *, *, #8821, .F. ) ;
#17428 = CARTESIAN_POINT ( 'NONE',  ( -24.36724102301519324, 2.559142463805198719, -12.49991998443061725 ) ) ;
#17429 = FACE_OUTER_BOUND ( 'NONE', #15475, .T. ) ;
#17430 = EDGE_CURVE ( 'NONE', #20723, #9936, #13511, .T. ) ;
#17431 = DIRECTION ( 'NONE',  ( 0.000000000000000000, 0.000000000000000000, -1.000000000000000000 ) ) ;
#17432 = CARTESIAN_POINT ( 'NONE',  ( -0.2217825122820056838, 6.780516198057334520, 1.739291495566667844 ) ) ;
#17433 = FACE_BOUND ( 'NONE', #23315, .T. ) ;
#17434 = CARTESIAN_POINT ( 'NONE',  ( -18.11469101799999848, 6.086102628551000038, 9.654141096248000764 ) ) ;
#17435 = CARTESIAN_POINT ( 'NONE',  ( 15.77981375731000036, 8.935760978467000015, -2.138706884349000248 ) ) ;
#17436 = DIRECTION ( 'NONE',  ( -0.6979779633368832226, -0.7161192377642821016, 2.278080596574945599E-09 ) ) ;
#17437 = ORIENTED_EDGE ( 'NONE', *, *, #12545, .T. ) ;
#17438 = CARTESIAN_POINT ( 'NONE',  ( 20.73762270046331579, -4.635149380793306406, -8.041800740487824228 ) ) ;
#17439 = CARTESIAN_POINT ( 'NONE',  ( -4.000000000000000000, 29.91693820796410108, 1.184172465503444904 ) ) ;
#17440 = DIRECTION ( 'NONE',  ( 0.000000000000000000, 0.000000000000000000, -1.000000000000000000 ) ) ;
#17441 = CARTESIAN_POINT ( 'NONE',  ( 2.374403550057654577, 13.96633455033458659, -5.646771293307399908 ) ) ;
#17442 = AXIS2_PLACEMENT_3D ( 'NONE', #20233, #20577, #3637 ) ;
#17443 = EDGE_LOOP ( 'NONE', ( #19172, #9769, #13712 ) ) ;
#17444 = CARTESIAN_POINT ( 'NONE',  ( 0.5251751504343997734, 13.80000824378999091, -6.149280467907001224 ) ) ;
#17445 = CARTESIAN_POINT ( 'NONE',  ( 19.60998953592000049, -11.09065046613000050, -1.415985076781999918 ) ) ;
#17446 = DIRECTION ( 'NONE',  ( -1.000000000000000000, 0.000000000000000000, 0.000000000000000000 ) ) ;
#17447 = CARTESIAN_POINT ( 'NONE',  ( 11.45478115325733448, -3.141659414319388777, 12.49993290927351453 ) ) ;
#17448 = CARTESIAN_POINT ( 'NONE',  ( 14.05762072145689245, -6.813077977408399377, -7.800977375048761431 ) ) ;
#17449 = CARTESIAN_POINT ( 'NONE',  ( -14.25623329758000146, -13.93375672974000068, 0.4323758512254999853 ) ) ;
#17450 = DIRECTION ( 'NONE',  ( 0.000000000000000000, 1.000000000000000000, 0.000000000000000000 ) ) ;
#17451 = CARTESIAN_POINT ( 'NONE',  ( 2.184465970885644648, 29.50086340285666964, -1.259047450927249345 ) ) ;
#17452 = VERTEX_POINT ( 'NONE', #3041 ) ;
#17453 = DIRECTION ( 'NONE',  ( 1.000000000000000000, 0.000000000000000000, 0.000000000000000000 ) ) ;
#17454 = CARTESIAN_POINT ( 'NONE',  ( 11.36701043060094563, -9.445581393775620782, 8.639701956158534202 ) ) ;
#17455 = ORIENTED_EDGE ( 'NONE', *, *, #22450, .F. ) ;
#17456 = DIRECTION ( 'NONE',  ( 0.000000000000000000, 1.000000000000000000, 0.000000000000000000 ) ) ;
#17457 = CARTESIAN_POINT ( 'NONE',  ( 1.536366799937304295, 28.51753006952333536, 1.999167105995438121 ) ) ;
#17458 = CARTESIAN_POINT ( 'NONE',  ( -3.128506986885329688, 13.13341830447926917, 5.987348177181893938 ) ) ;
#17459 = CARTESIAN_POINT ( 'NONE',  ( 6.145347424894735511, 14.16395735418471702, -0.1681360381669483595 ) ) ;
#17460 = CARTESIAN_POINT ( 'NONE',  ( 1.709999999999999964, 13.00000000000000000, 7.500000000000000000 ) ) ;
#17461 = B_SPLINE_CURVE_WITH_KNOTS ( 'NONE', 3,
 ( #15713, #21432, #6643, #14038 ),
 .UNSPECIFIED., .F., .F.,
 ( 4, 4 ),
 ( 0.000000000000000000, 1.000000000000000000 ),
 .UNSPECIFIED. ) ;
#17462 = CARTESIAN_POINT ( 'NONE',  ( -0.2814148094397999622, 26.38669433609999970, -2.857252503208999705 ) ) ;
#17463 = VERTEX_POINT ( 'NONE', #14049 ) ;
#17464 = ORIENTED_EDGE ( 'NONE', *, *, #6460, .T. ) ;
#17465 = CARTESIAN_POINT ( 'NONE',  ( -13.99999999999999822, -5.054693537803610859, -8.380144158881588368 ) ) ;
#17466 = CYLINDRICAL_SURFACE ( 'NONE', #10154, 7.000000000000000000 ) ;
#17467 = DIRECTION ( 'NONE',  ( -1.000000000000000000, 0.000000000000000000, 0.000000000000000000 ) ) ;
#17468 = ADVANCED_FACE ( 'NONE', ( #14295 ), #21320, .F. ) ;
#17469 = ORIENTED_EDGE ( 'NONE', *, *, #17841, .F. ) ;
#17470 = CARTESIAN_POINT ( 'NONE',  ( 0.000000000000000000, 13.00000000000000000, 0.000000000000000000 ) ) ;
#17471 = DIRECTION ( 'NONE',  ( 0.000000000000000000, 1.000000000000000000, 0.000000000000000000 ) ) ;
#17472 = CARTESIAN_POINT ( 'NONE',  ( 15.14846033456440644, 7.199530315733793984, 7.418362551489144252 ) ) ;
#17473 = CARTESIAN_POINT ( 'NONE',  ( -14.40415622949000074, -1.547762950494000034, 10.89277918470000017 ) ) ;
#17474 = CARTESIAN_POINT ( 'NONE',  ( -0.9520732478256999087, 29.36900269487000159, 2.155299678714000411 ) ) ;
#17475 = CARTESIAN_POINT ( 'NONE',  ( -21.23063454076328327, -10.41326765124834708, -1.537861545000790864 ) ) ;
#17476 = CARTESIAN_POINT ( 'NONE',  ( -15.27086614641999951, -1.548365329537000123, -11.22688807791999999 ) ) ;
#17477 = AXIS2_PLACEMENT_3D ( 'NONE', #18477, #7442, #22216 ) ;
#17478 = CARTESIAN_POINT ( 'NONE',  ( -1.202564115966959557, 29.52878198405490906, 1.797833957355160717 ) ) ;
#17479 = ORIENTED_EDGE ( 'NONE', *, *, #13548, .T. ) ;
#17480 = CARTESIAN_POINT ( 'NONE',  ( -2.306707304653000001, 25.24613028134000103, 0.4431434081515999712 ) ) ;
#17481 = CARTESIAN_POINT ( 'NONE',  ( -17.06754031676047134, 4.332830716336383503, -9.488203514064112554 ) ) ;
#17482 = B_SPLINE_CURVE_WITH_KNOTS ( 'NONE', 3,
 ( #16423, #14498, #11104, #18152, #18026, #20082, #8940, #9290, #16664, #70 ),
 .UNSPECIFIED., .F., .F.,
 ( 4, 2, 2, 2, 4 ),
 ( 4.238274817591080088E-05, 0.0007680267671880953821, 0.001493670786200280119, 0.002219314805212464423, 0.002944958824224649160 ),
 .UNSPECIFIED. ) ;
#17483 = VERTEX_POINT ( 'NONE', #12243 ) ;
#17484 = CARTESIAN_POINT ( 'NONE',  ( -10.90000000000000036, -7.100000000000000533, -1.377928257607000217E-10 ) ) ;
#17485 = CARTESIAN_POINT ( 'NONE',  ( 6.533539489258001431, 13.52322660849999991, -1.215173520708999977 ) ) ;
#17486 = CARTESIAN_POINT ( 'NONE',  ( 11.99999999999999822, -3.638042036673571733, -8.209236114036826848 ) ) ;
#17487 = AXIS2_PLACEMENT_3D ( 'NONE', #22056, #5465, #12847 ) ;
#17488 = CARTESIAN_POINT ( 'NONE',  ( 0.000000000000000000, 21.87500000000000000, 0.000000000000000000 ) ) ;
#17489 = CARTESIAN_POINT ( 'NONE',  ( 18.79425158531000051, -6.072333155528000681, 7.996935486658999892 ) ) ;
#17490 = EDGE_LOOP ( 'NONE', ( #1135, #16314, #23744, #22794, #8850 ) ) ;
#17491 = CARTESIAN_POINT ( 'NONE',  ( -1.999167105995452998, 27.11666666666667425, -1.536366799937284089 ) ) ;
#17492 = DIRECTION ( 'NONE',  ( 0.000000000000000000, 0.000000000000000000, -1.000000000000000000 ) ) ;
#17493 = EDGE_CURVE ( 'NONE', #14758, #14191, #8727, .T. ) ;
#17494 = EDGE_LOOP ( 'NONE', ( #14093, #1947, #17262 ) ) ;
#17496 = B_SPLINE_CURVE_WITH_KNOTS ( 'NONE', 3,
 ( #15445, #19079, #21023, #15199, #18726 ),
 .UNSPECIFIED., .F., .F.,
 ( 4, 1, 4 ),
 ( 0.000000000000000000, 0.5000000000000000000, 1.000000000000000000 ),
 .UNSPECIFIED. ) ;
#17495 = CARTESIAN_POINT ( 'NONE',  ( -14.25243324638999809, -6.216878364870000340, 12.50000000000000000 ) ) ;
#17497 = CARTESIAN_POINT ( 'NONE',  ( 12.28779254560826395, 7.992768853863905676, 11.15614400023877906 ) ) ;
#17498 = CARTESIAN_POINT ( 'NONE',  ( -23.16929462096833703, 9.265295224643226746, 1.607743681355135241E-05 ) ) ;
#17499 = TOROIDAL_SURFACE ( 'NONE', #22143, 7.200000000000000178, 0.1000000000000000056 ) ;
#17500 = DIRECTION ( 'NONE',  ( 0.000000000000000000, -1.000000000000000000, 0.000000000000000000 ) ) ;
#17501 = CARTESIAN_POINT ( 'NONE',  ( 18.39137590704549297, 8.967538887471349085, -5.308501318233523669 ) ) ;
#17502 = CARTESIAN_POINT ( 'NONE',  ( 11.99999999999999645, -6.864517642019856147, -7.017967020444166870 ) ) ;
#17503 = CARTESIAN_POINT ( 'NONE',  ( -14.50000017458758705, 10.95512910623404856, -6.025157725042314283 ) ) ;
#17504 = CARTESIAN_POINT ( 'NONE',  ( 19.17012474526000076, -11.07867377307000112, -1.414454806264999975 ) ) ;
#17505 = DIRECTION ( 'NONE',  ( 0.000000000000000000, -1.000000000000000000, 0.000000000000000000 ) ) ;
#17506 = CARTESIAN_POINT ( 'NONE',  ( -3.738560243459424282, 14.17257416838673301, -4.872431394003077898 ) ) ;
#17507 = DIRECTION ( 'NONE',  ( -1.000000000000000000, 0.000000000000000000, 0.000000000000000000 ) ) ;
#17508 = ADVANCED_FACE ( 'NONE', ( #19865 ), #961, .T. ) ;
#17509 = CARTESIAN_POINT ( 'NONE',  ( -1.706528196843968725, 30.28866702718950776, 1.336746582747178502 ) ) ;
#17510 = EDGE_LOOP ( 'NONE', ( #13673, #18934, #20414, #5935 ) ) ;
#17511 = CARTESIAN_POINT ( 'NONE',  ( 22.40534660507999831, -6.082126118738999665, 9.068436681591000692 ) ) ;
#17512 = CARTESIAN_POINT ( 'NONE',  ( 23.19333426533477649, -9.788860759441813997, -4.063454424824834987 ) ) ;
#17513 = CARTESIAN_POINT ( 'NONE',  ( -2.184465970885641983, 27.50086340285666608, 1.259047450927253564 ) ) ;
#17514 = CARTESIAN_POINT ( 'NONE',  ( 1.526275108040723971, 24.72983374295983339, 1.538304002670136894 ) ) ;
#17515 = CARTESIAN_POINT ( 'NONE',  ( 0.000000000000000000, 20.10000000000000142, -3.000000000000416112 ) ) ;
#17516 = TOROIDAL_SURFACE ( 'NONE', #22529, 14.44999999999999929, 3.850000000000000089 ) ;
#17517 = CARTESIAN_POINT ( 'NONE',  ( -4.788527363615000532, 12.45561528826001485, -1.254325367001999147 ) ) ;
#17518 = ORIENTED_EDGE ( 'NONE', *, *, #11166, .T. ) ;
#17519 = ADVANCED_FACE ( 'NONE', ( #15726 ), #21208, .F. ) ;
#17520 = LINE ( 'NONE', #8441, #6618 ) ;
#17521 = DIRECTION ( 'NONE',  ( 0.000000000000000000, 0.000000000000000000, 1.000000000000000000 ) ) ;
#17522 = CARTESIAN_POINT ( 'NONE',  ( -0.6943634456196157156, 27.47093684869671293, -2.086060929983299950 ) ) ;
#17523 = PRODUCT_CONTEXT ( 'NONE', #6482, 'mechanical' ) ;
#17524 = ORIENTED_EDGE ( 'NONE', *, *, #23005, .T. ) ;
#17525 = ADVANCED_FACE ( 'NONE', ( #23213, #8456, #3136 ), #928, .F. ) ;
#17526 = ORIENTED_EDGE ( 'NONE', *, *, #6046, .T. ) ;
#17527 = CARTESIAN_POINT ( 'NONE',  ( 17.29858103379666545, 1.193049601325067988, -9.115197396075636505 ) ) ;
#17528 = CARTESIAN_POINT ( 'NONE',  ( 15.53006424931000140, -9.332187211223001100, 5.252733788881000621 ) ) ;
#17529 = CARTESIAN_POINT ( 'NONE',  ( -24.48870547333000047, 5.980820260656999565, -8.894311732265000714 ) ) ;
#17530 = CARTESIAN_POINT ( 'NONE',  ( -18.13280809636999891, -10.33926822794999900, 0.2327566560484999880 ) ) ;
#17531 = CARTESIAN_POINT ( 'NONE',  ( -0.6838519464012248195, 24.63336607546796841, 4.223839491855484241 ) ) ;
#17532 = CARTESIAN_POINT ( 'NONE',  ( 15.26124951745999958, 1.362798856695000005, -9.630360975484999031 ) ) ;
#17533 = FACE_BOUND ( 'NONE', #18198, .T. ) ;
#17534 = FACE_OUTER_BOUND ( 'NONE', #14496, .T. ) ;
#17535 = EDGE_CURVE ( 'NONE', #9272, #10321, #17418, .T. ) ;
#17536 = CARTESIAN_POINT ( 'NONE',  ( 6.162318803892000041, 13.65473356602000088, -2.204421525222999723 ) ) ;
#17537 = ORIENTED_EDGE ( 'NONE', *, *, #10428, .T. ) ;
#17538 = CARTESIAN_POINT ( 'NONE',  ( -0.7737468029517903245, 13.71960327777151356, 6.079035818031503169 ) ) ;
#17539 = CARTESIAN_POINT ( 'NONE',  ( -2.866097959738999723, 27.26750240009999970, 0.1690226414555000001 ) ) ;
#17540 = CARTESIAN_POINT ( 'NONE',  ( -4.175107824646003607, 12.32875441307999864, 2.224447038902001239 ) ) ;
#17541 = CARTESIAN_POINT ( 'NONE',  ( -19.31991243917331857, 8.928523062339214889, -2.399343565118006172 ) ) ;
#17542 = CARTESIAN_POINT ( 'NONE',  ( -14.46243031116633659, 2.866065099209276656, -8.600290833557869163 ) ) ;
#17543 = CARTESIAN_POINT ( 'NONE',  ( -22.58353710275999759, 6.208000067599999561, -9.226852243910000695 ) ) ;
#17544 = DIRECTION ( 'NONE',  ( -1.000000000000000000, 0.000000000000000000, 0.000000000000000000 ) ) ;
#17545 = VERTEX_POINT ( 'NONE', #15822 ) ;
#17546 = CARTESIAN_POINT ( 'NONE',  ( 0.000000000000000000, 17.00000000000000000, 0.000000000000000000 ) ) ;
#17547 = CARTESIAN_POINT ( 'NONE',  ( 4.750000000000000000, 20.10000000000000142, 0.000000000000000000 ) ) ;
#17548 = CARTESIAN_POINT ( 'NONE',  ( 3.197564234074002254, 13.68604480655000621, 5.201785757272003430 ) ) ;
#17549 = CARTESIAN_POINT ( 'NONE',  ( -1.183772340028661274, 6.880224493752307602, 1.289604923395413438 ) ) ;
#17550 = DIRECTION ( 'NONE',  ( -1.000000000000000000, 0.000000000000000000, 0.000000000000000000 ) ) ;
#17551 = EDGE_CURVE ( 'NONE', #20493, #21674, #21534, .T. ) ;
#17552 = EDGE_CURVE ( 'NONE', #12256, #2155, #7712, .T. ) ;
#17553 = LINE ( 'NONE', #8347, #5961 ) ;
#17554 = CARTESIAN_POINT ( 'NONE',  ( -18.52095171394000062, 10.52702611403999988, -4.436598560839000172 ) ) ;
#17555 = CARTESIAN_POINT ( 'NONE',  ( 13.69575125731000043, 3.560502093102000387, -8.410767149301999979 ) ) ;
#17556 = CARTESIAN_POINT ( 'NONE',  ( -1.999167105995447224, 27.28333333333333499, 1.536366799937292305 ) ) ;
#17557 = AXIS2_PLACEMENT_3D ( 'NONE', #23320, #4696, #14370 ) ;
#17558 = EDGE_LOOP ( 'NONE', ( #4743, #2563, #9467, #23607, #3115, #10736 ) ) ;
#17559 = B_SPLINE_CURVE_WITH_KNOTS ( 'NONE', 3,
 ( #13307, #4113, #18887, #15358, #9685, #6039, #13427, #20947, #22748, #6167, #17679, #19621 ),
 .UNSPECIFIED., .F., .F.,
 ( 4, 1, 1, 1, 1, 2, 2, 4 ),
 ( 0.000000000000000000, 0.2499999999999964473, 0.3749999999999947820, 0.4374999999999936717, 0.4687499999999933387, 0.4843749999999933942, 0.4999999999999934497, 1.000000000000000000 ),
 .UNSPECIFIED. ) ;
#17560 = CARTESIAN_POINT ( 'NONE',  ( -22.49384739520191800, 2.420755952246590237, 9.006231210083697647 ) ) ;
#17561 = CARTESIAN_POINT ( 'NONE',  ( -0.2155490653164000014, 30.96541312239999755, -2.523581531315999715 ) ) ;
#17562 = CARTESIAN_POINT ( 'NONE',  ( -12.41173981160000039, 6.613190111079999767, -13.46349570337000046 ) ) ;
#17563 = CARTESIAN_POINT ( 'NONE',  ( 2.053618936107731052, 13.89760215911831942, -5.770478405391227916 ) ) ;
#17564 = ORIENTED_EDGE ( 'NONE', *, *, #4955, .F. ) ;
#17565 = CARTESIAN_POINT ( 'NONE',  ( 4.566396831513001686, 14.20660692728000285, -4.011688757825002227 ) ) ;
#17566 =( NAMED_UNIT ( * ) PLANE_ANGLE_UNIT ( ) SI_UNIT ( $, .RADIAN. ) );
#17567 = CARTESIAN_POINT ( 'NONE',  ( -2.740231804698999962, 29.76618196464000121, -0.1726680830762000185 ) ) ;
#17568 = EDGE_CURVE ( 'NONE', #23444, #10297, #10827, .T. ) ;
#17569 = DIRECTION ( 'NONE',  ( -0.000000000000000000, 1.000000000000000000, 0.000000000000000000 ) ) ;
#17570 = ADVANCED_FACE ( 'NONE', ( #12333 ), #19837, .T. ) ;
#17571 = CARTESIAN_POINT ( 'NONE',  ( 15.61874380413824781, -10.39027652322779183, 0.2460966605066790269 ) ) ;
#17572 = PLANE ( 'NONE',  #14518 ) ;
#17573 = DIRECTION ( 'NONE',  ( 1.000000000000000000, 0.000000000000000000, 0.000000000000000000 ) ) ;
#17574 = CIRCLE ( 'NONE', #7117, 10.59999999999999964 ) ;
#17575 = DIRECTION ( 'NONE',  ( 0.000000000000000000, -1.000000000000000000, 0.000000000000000000 ) ) ;
#17576 = ORIENTED_EDGE ( 'NONE', *, *, #23915, .T. ) ;
#17577 = CARTESIAN_POINT ( 'NONE',  ( -24.50000000000000000, -5.567336242322655337, -8.985968813393915511 ) ) ;
#17578 = CARTESIAN_POINT ( 'NONE',  ( 1.768240990936880142, 24.49990546444021078, -1.767061324597003713 ) ) ;
#17579 = ORIENTED_EDGE ( 'NONE', *, *, #3143, .F. ) ;
#17580 = CARTESIAN_POINT ( 'NONE',  ( -5.684582646178887977, 16.21817490744206580, -2.283151055710457733 ) ) ;
#17581 = CARTESIAN_POINT ( 'NONE',  ( 2.079313456931997539, 24.24494735708400839, -0.6989243223293186702 ) ) ;
#17582 = CARTESIAN_POINT ( 'NONE',  ( -0.6548632618487933987, 12.81818377440604273, 6.635320921360461810 ) ) ;
#17583 = CIRCLE ( 'NONE', #17969, 12.50000000000000178 ) ;
#17584 = CARTESIAN_POINT ( 'NONE',  ( 6.144969876179364299, 14.16671624030418108, -0.1596052567943958833 ) ) ;
#17585 = FACE_OUTER_BOUND ( 'NONE', #3873, .T. ) ;
#17586 = CARTESIAN_POINT ( 'NONE',  ( 24.37713355803437665, -2.989142673506740788, -12.50000000000000355 ) ) ;
#17587 = ORIENTED_EDGE ( 'NONE', *, *, #9534, .F. ) ;
#17588 = FACE_OUTER_BOUND ( 'NONE', #21287, .T. ) ;
#17589 = CONICAL_SURFACE ( 'NONE', #23380, 2.949999959913000236, 0.7853981633972997312 ) ;
#17590 = CARTESIAN_POINT ( 'NONE',  ( 0.000000000000000000, 18.27087121525220681, 0.000000000000000000 ) ) ;
#17591 = CARTESIAN_POINT ( 'NONE',  ( -10.35615758860000035, 0.000000000000000000, -7.000000000000000000 ) ) ;
#17592 =( BOUNDED_SURFACE ( )  B_SPLINE_SURFACE ( 3, 3, ( 
 ( #20420, #14376, #10632, #1547, #1421, #21770, #5182, #16301, #3486, #18252, #1654 ),
 ( #16415, #23805, #7213, #22000, #5413, #20185, #14718, #3595, #10978, #1773, #23926 ),
 ( #22114, #17255, #3947, #654, #7566, #8058, #11342, #15070, #22464, #20899, #5760 ),
 ( #2359, #15430, #22816, #15186, #7936, #18712, #11224, #6232, #5874, #13613, #174 ) ),
 .UNSPECIFIED., .F., .F., .T. ) 
 B_SPLINE_SURFACE_WITH_KNOTS ( ( 4, 4 ),
 ( 4, 1, 1, 1, 1, 1, 1, 1, 4 ),
 ( 0.000000000000000000, 1.000000000000000000 ),
 ( 0.6777550477067999513, 0.7077183713728000258, 0.7630935829821999805, 0.8160430438097999728, 0.8631236143084000112, 0.9059812851685999924, 0.9500234102994999930, 1.000000000000000000, 1.005511424025000045 ),
 .UNSPECIFIED. ) 
 GEOMETRIC_REPRESENTATION_ITEM ( )  RATIONAL_B_SPLINE_SURFACE ( (
 ( 1.339324717273000065, 1.339324717273000065, 1.339324717273000065, 1.339324717273000065, 1.339324717273000065, 1.339324717273000065, 1.339324717273000065, 1.339324717273000065, 1.339324717273000065, 1.339324717273000065, 1.339324717273000065),
 ( 0.8868917609088999843, 0.8868917609088999843, 0.8868917609088999843, 0.8868917609088999843, 0.8868917609088999843, 0.8868917609088999843, 0.8868917609088999843, 0.8868917609088999843, 0.8868917609088999843, 0.8868917609088999843, 0.8868917609088999843),
 ( 0.8868917609088999843, 0.8868917609088999843, 0.8868917609088999843, 0.8868917609088999843, 0.8868917609088999843, 0.8868917609088999843, 0.8868917609088999843, 0.8868917609088999843, 0.8868917609088999843, 0.8868917609088999843, 0.8868917609088999843),
 ( 1.339324717273000065, 1.339324717273000065, 1.339324717273000065, 1.339324717273000065, 1.339324717273000065, 1.339324717273000065, 1.339324717273000065, 1.339324717273000065, 1.339324717273000065, 1.339324717273000065, 1.339324717273000065) ) ) 
 REPRESENTATION_ITEM ( '' )  SURFACE ( )  );
#17593 = EDGE_LOOP ( 'NONE', ( #16030, #16289, #6406, #13209 ) ) ;
#17594 = CARTESIAN_POINT ( 'NONE',  ( -24.44714577827999946, -5.477234815341000207, -9.903190068764999410 ) ) ;
#17595 = CARTESIAN_POINT ( 'NONE',  ( -2.246347731941017223, 24.65365226805931087, -5.222125272214524731E-08 ) ) ;
#17596 = PLANE ( 'NONE',  #4884 ) ;
#17597 = CARTESIAN_POINT ( 'NONE',  ( 15.04368363787946805, 9.348761382856489277, 4.437686386494108071 ) ) ;
#17598 =( GEOMETRIC_REPRESENTATION_CONTEXT ( 3 ) GLOBAL_UNCERTAINTY_ASSIGNED_CONTEXT ( ( #3395 ) ) GLOBAL_UNIT_ASSIGNED_CONTEXT ( ( #4305, #11695, #7817 ) ) REPRESENTATION_CONTEXT ( 'NONE', 'WORKASPACE' ) );
#17599 = CARTESIAN_POINT ( 'NONE',  ( -16.89940092177999986, 10.96253337826999896, -1.543077568198000016 ) ) ;
#17600 = CARTESIAN_POINT ( 'NONE',  ( 4.834858920412084871, 12.45115190511012138, -0.1243179763900293527 ) ) ;
#17601 = CARTESIAN_POINT ( 'NONE',  ( -19.91814312763024475, 0.2067535327646641552, 10.49027380322098324 ) ) ;
#17602 = CARTESIAN_POINT ( 'NONE',  ( -0.5801434548614997633, 11.64265918162999114, -4.731509157062997240 ) ) ;
#17603 = FACE_BOUND ( 'NONE', #9613, .T. ) ;
#17604 = CARTESIAN_POINT ( 'NONE',  ( -2.160954628185623783, 29.42171253127930797, 0.3064887866906846892 ) ) ;
#17605 = ORIENTED_EDGE ( 'NONE', *, *, #9381, .F. ) ;
#17606 = CARTESIAN_POINT ( 'NONE',  ( 2.346791958811000001, 24.82734368833999739, -0.09920819339686001714 ) ) ;
#17607 = CARTESIAN_POINT ( 'NONE',  ( -17.00966196906368921, 6.126770844779409586, -8.438622901460794523 ) ) ;
#17608 = B_SPLINE_CURVE_WITH_KNOTS ( 'NONE', 3,
 ( #11985, #12107, #13545, #22863 ),
 .UNSPECIFIED., .F., .F.,
 ( 4, 4 ),
 ( 0.8463849510497769568, 1.000000000000000000 ),
 .UNSPECIFIED. ) ;
#17609 = ORIENTED_EDGE ( 'NONE', *, *, #19165, .F. ) ;
#17610 = CARTESIAN_POINT ( 'NONE',  ( -3.574277709506242531E-06, 28.66502397170827621, 2.098898342233183723 ) ) ;
#17611 = CARTESIAN_POINT ( 'NONE',  ( 6.132481042133004046, 14.49467011299998909, -0.0001351461492217999522 ) ) ;
#17612 = CARTESIAN_POINT ( 'NONE',  ( -4.633248246530266456, 13.46040479489061248, -5.211335153246753116 ) ) ;
#17613 = CARTESIAN_POINT ( 'NONE',  ( 23.99062354302999722, 6.216878364870000340, -12.50000000000000000 ) ) ;
#17614 = CARTESIAN_POINT ( 'NONE',  ( 18.35550158530999809, 7.854726640733000309, 6.622681824707000509 ) ) ;
#17615 = ORIENTED_EDGE ( 'NONE', *, *, #21353, .T. ) ;
#17616 = CARTESIAN_POINT ( 'NONE',  ( -10.04281598263999875, 1.347635823622999967E-14, 0.000000000000000000 ) ) ;
#17617 = CARTESIAN_POINT ( 'NONE',  ( 4.849999930150000083, 12.54999993386000057, -7.274541077495999001E-07 ) ) ;
#17618 = DIRECTION ( 'NONE',  ( 0.000000000000000000, -1.000000000000000000, 0.000000000000000000 ) ) ;
#17619 = ORIENTED_EDGE ( 'NONE', *, *, #17065, .T. ) ;
#17620 = CARTESIAN_POINT ( 'NONE',  ( -11.00000000000000000, 7.200000000000000178, 0.000000000000000000 ) ) ;
#17621 = DIRECTION ( 'NONE',  ( 0.000000000000000000, 1.000000000000000000, 0.000000000000000000 ) ) ;
#17622 = CARTESIAN_POINT ( 'NONE',  ( -7.834000000000000519, -10.59999999999999964, 0.000000000000000000 ) ) ;
#17623 = AXIS2_PLACEMENT_3D ( 'NONE', #11722, #22489, #8210 ) ;
#17624 = CARTESIAN_POINT ( 'NONE',  ( -3.304996520289660733, 26.37418302490023692, 2.710661522857508388 ) ) ;
#17625 = CARTESIAN_POINT ( 'NONE',  ( 17.66124585261385604, -10.36187385480047851, -0.9006329633823950687 ) ) ;
#17626 = CARTESIAN_POINT ( 'NONE',  ( -23.76320767499999675, 6.967090338468000077, 12.06686491509000092 ) ) ;
#17627 = CARTESIAN_POINT ( 'NONE',  ( 13.21250000000000036, 0.000000000000000000, 0.000000000000000000 ) ) ;
#17628 = CARTESIAN_POINT ( 'NONE',  ( 21.33576293477999641, -7.518524484350999515, -8.339206206814999689 ) ) ;
#17629 = CARTESIAN_POINT ( 'NONE',  ( 0.000000000000000000, 28.15000000000000213, 0.000000000000000000 ) ) ;
#17630 = CARTESIAN_POINT ( 'NONE',  ( 12.52688711657000020, 6.216878364870000340, -12.50000000000000000 ) ) ;
#17631 = CARTESIAN_POINT ( 'NONE',  ( -2.140916772114409117, 30.22093133680311183, 0.2897247076014631273 ) ) ;
#17632 = ORIENTED_EDGE ( 'NONE', *, *, #22973, .T. ) ;
#17633 = CARTESIAN_POINT ( 'NONE',  ( 19.69983353523999980, 6.514647315076000034, -8.669487664655999737 ) ) ;
#17634 = CARTESIAN_POINT ( 'NONE',  ( 3.999895459877826465, 28.20780860099995024, -1.909390889640790512 ) ) ;
#17635 = CARTESIAN_POINT ( 'NONE',  ( -1.259047450927242018, 27.56753006952333607, 2.184465970885648201 ) ) ;
#17636 = EDGE_CURVE ( 'NONE', #17401, #7987, #929, .T. ) ;
#17637 = CARTESIAN_POINT ( 'NONE',  ( -2.135131282218049265, 24.38894026383828972, -0.7200268973484618140 ) ) ;
#17638 = CIRCLE ( 'NONE', #2944, 7.000000000000000000 ) ;
#17639 = CARTESIAN_POINT ( 'NONE',  ( 4.912321670294291565, 14.34861163470688084, 3.825009897921954227 ) ) ;
#17640 = ORIENTED_EDGE ( 'NONE', *, *, #6076, .F. ) ;
#17641 = CARTESIAN_POINT ( 'NONE',  ( -14.86532595926124500, 9.166658182833229418, -4.831506234239814290 ) ) ;
#17642 = CARTESIAN_POINT ( 'NONE',  ( -4.000000000000000000, 24.50000000000000000, 0.000000000000000000 ) ) ;
#17643 = CARTESIAN_POINT ( 'NONE',  ( 30.87226923053214378, 27.01856778792605240, -2.673746900119611247 ) ) ;
#17644 = DIRECTION ( 'NONE',  ( 1.000000000000000000, 0.000000000000000000, 0.000000000000000000 ) ) ;
#17645 = CARTESIAN_POINT ( 'NONE',  ( -14.38789255203824879, -4.127795921257689571, -12.49979377837149208 ) ) ;
#17646 = EDGE_CURVE ( 'NONE', #3203, #15451, #16216, .T. ) ;
#17647 = ORIENTED_EDGE ( 'NONE', *, *, #9923, .T. ) ;
#17648 = DIRECTION ( 'NONE',  ( 1.000000000000000000, 0.000000000000000000, 0.000000000000000000 ) ) ;
#17649 = CARTESIAN_POINT ( 'NONE',  ( -5.372805085453999929, 16.07374366015000078, -2.940844016990000309 ) ) ;
#17650 = CARTESIAN_POINT ( 'NONE',  ( -24.38011137294000008, 0.4010730224961999713, -11.22689660418999935 ) ) ;
#17651 = CARTESIAN_POINT ( 'NONE',  ( -19.75785088013000035, -8.381234170548999884, -6.136494560970000123 ) ) ;
#17652 = CARTESIAN_POINT ( 'NONE',  ( -6.063697158388001718, 15.62880598230002249, 1.260709251179999324 ) ) ;
#17653 = CARTESIAN_POINT ( 'NONE',  ( 19.72999951746000136, 0.8733432563274000637, 9.811130420370998806 ) ) ;
#17654 = CARTESIAN_POINT ( 'NONE',  ( 0.8375244288382391877, 28.35398498632677189, -2.004067736020587187 ) ) ;
#17655 = CIRCLE ( 'NONE', #2566, 13.75000000000000000 ) ;
#17656 = B_SPLINE_CURVE_WITH_KNOTS ( 'NONE', 3,
 ( #15108, #9791, #13418, #6393, #15225, #19110, #4593, #572, #17428, #17300, #8223, #16935, #20696, #6156 ),
 .UNSPECIFIED., .F., .F.,
 ( 4, 2, 2, 2, 2, 2, 4 ),
 ( 0.000000000000000000, 0.2500000000000001110, 0.3750000000000001110, 0.5000000000000001110, 0.6250000000000000000, 0.7500000000000000000, 1.000000000000000000 ),
 .UNSPECIFIED. ) ;
#17657 = AXIS2_PLACEMENT_3D ( 'NONE', #9992, #2853, #6837 ) ;
#17658 = CARTESIAN_POINT ( 'NONE',  ( 20.76146583675999935, 3.250716185844000350, -9.124108739569999571 ) ) ;
#17659 = DIRECTION ( 'NONE',  ( -1.000000000000000000, 0.000000000000000000, 0.000000000000000000 ) ) ;
#17660 = ORIENTED_EDGE ( 'NONE', *, *, #7834, .T. ) ;
#17661 = CARTESIAN_POINT ( 'NONE',  ( 1.413067587578629380, 13.78907544507517535, 5.959893886319711953 ) ) ;
#17662 = CARTESIAN_POINT ( 'NONE',  ( 0.1921407682535675732, 24.77615385734275932, 2.130435955740220155 ) ) ;
#17663 = CARTESIAN_POINT ( 'NONE',  ( -19.88678743917331815, -5.642442153596147314, -7.342323539242457286 ) ) ;
#17664 = EDGE_CURVE ( 'NONE', #17201, #3390, #6990, .T. ) ;
#17665 = CARTESIAN_POINT ( 'NONE',  ( 1.798742361870000028, 27.50937716035999969, -1.662740336262000129 ) ) ;
#17666 = AXIS2_PLACEMENT_3D ( 'NONE', #13872, #2862, #19818 ) ;
#17667 = CARTESIAN_POINT ( 'NONE',  ( 0.000000000000000000, 24.65000000000000213, 0.000000000000000000 ) ) ;
#17668 = ORIENTED_EDGE ( 'NONE', *, *, #7146, .T. ) ;
#17669 = CARTESIAN_POINT ( 'NONE',  ( 15.90028936713000185, 9.079314476020000413, 0.000000000000000000 ) ) ;
#17670 = CARTESIAN_POINT ( 'NONE',  ( 2.331536102386086107, 11.71301274535795933, -4.220455149562390318 ) ) ;
#17671 = CARTESIAN_POINT ( 'NONE',  ( 4.166162063823999340, 14.03319894470998364, 4.455060026797000639 ) ) ;
#17672 = AXIS2_PLACEMENT_3D ( 'NONE', #21704, #10802, #16105 ) ;
#17673 = CARTESIAN_POINT ( 'NONE',  ( 0.1325762199310360212, 30.23768260327807411, 2.274129417085968718 ) ) ;
#17674 = DIRECTION ( 'NONE',  ( 0.000000000000000000, -1.000000000000000000, 0.000000000000000000 ) ) ;
#17675 = EDGE_CURVE ( 'NONE', #15250, #3998, #13898, .T. ) ;
#17676 = CARTESIAN_POINT ( 'NONE',  ( -11.51617721169000141, -15.07264118231999994, 3.899284990158000230 ) ) ;
#17677 = CARTESIAN_POINT ( 'NONE',  ( -17.30216962611999776, -8.848728181206000798, -7.171245711509000920 ) ) ;
#17678 = CARTESIAN_POINT ( 'NONE',  ( 13.06406392131000160, -4.637122060904999898, 8.435305548789999719 ) ) ;
#17679 = CARTESIAN_POINT ( 'NONE',  ( 24.50000000000000000, 11.33659675998026728, -5.364438426793228132 ) ) ;
#17680 = ORIENTED_EDGE ( 'NONE', *, *, #20310, .F. ) ;
#17681 = DIRECTION ( 'NONE',  ( -1.000000000000000000, 0.000000000000000000, 0.000000000000000000 ) ) ;
#17682 = CARTESIAN_POINT ( 'NONE',  ( 1.375673147160000109, 30.52907988946000017, 1.895117694842000100 ) ) ;
#17683 = AXIS2_PLACEMENT_3D ( 'NONE', #10322, #3301, #21221 ) ;
#17684 = DIRECTION ( 'NONE',  ( -1.000000000000000000, 0.000000000000000000, 0.000000000000000000 ) ) ;
#17685 = CARTESIAN_POINT ( 'NONE',  ( -1.730145359313365550, 13.83619868571590672, -5.879316393191865942 ) ) ;
#17686 = ORIENTED_EDGE ( 'NONE', *, *, #1664, .T. ) ;
#17687 = CIRCLE ( 'NONE', #13795, 3.000000000000000000 ) ;
#17688 = EDGE_CURVE ( 'NONE', #19360, #16087, #6164, .T. ) ;
#17689 = CARTESIAN_POINT ( 'NONE',  ( 24.50000000000000000, 0.000000000000000000, 0.000000000000000000 ) ) ;
#17690 = DIRECTION ( 'NONE',  ( -1.000000000000000000, 0.000000000000000000, 0.000000000000000000 ) ) ;
#17691 = CARTESIAN_POINT ( 'NONE',  ( 0.000000000000000000, 18.50000000000000000, 0.000000000000000000 ) ) ;
#17692 = CARTESIAN_POINT ( 'NONE',  ( 0.000000000000000000, -1.550000000000000044, 0.000000000000000000 ) ) ;
#17693 = CARTESIAN_POINT ( 'NONE',  ( 14.72667347117745429, 10.36589271863794259, 0.2970802226479983266 ) ) ;
#17694 = AXIS2_PLACEMENT_3D ( 'NONE', #10825, #1250, #6816 ) ;
#17695 = CARTESIAN_POINT ( 'NONE',  ( -3.644446339697000159, 14.33206891720999998, 4.922772686299000000 ) ) ;
#17696 = DIRECTION ( 'NONE',  ( 1.000000000000000000, 0.000000000000000000, 0.000000000000000000 ) ) ;
#17697 = ADVANCED_FACE ( 'NONE', ( #17534 ), #8328, .T. ) ;
#17698 = CARTESIAN_POINT ( 'NONE',  ( -24.46742986864117597, -10.18447769902851263, 7.359979596114137657 ) ) ;
#17699 = VERTEX_POINT ( 'NONE', #13892 ) ;
#17700 = DIRECTION ( 'NONE',  ( 0.000000000000000000, -1.000000000000000000, 0.000000000000000000 ) ) ;
#17701 = ADVANCED_FACE ( 'NONE', ( #14494 ), #20070, .F. ) ;
#17702 = CARTESIAN_POINT ( 'NONE',  ( -19.10482910584000038, 1.458613477275000161E-14, 0.000000000000000000 ) ) ;
#17703 = ORIENTED_EDGE ( 'NONE', *, *, #15151, .T. ) ;
#17704 = CARTESIAN_POINT ( 'NONE',  ( -2.505762909214999556, 23.97700368146000116, 0.4461716537489999745 ) ) ;
#17705 = CARTESIAN_POINT ( 'NONE',  ( 0.000000000000000000, 28.00000000000000000, -2.400000000000455991 ) ) ;
#17706 = CARTESIAN_POINT ( 'NONE',  ( 3.696164193155713207, 13.26185372247518046, 5.697559243385613037 ) ) ;
#17707 = VECTOR ( 'NONE', #20435, 1000.000000000000000 ) ;
#17708 = CARTESIAN_POINT ( 'NONE',  ( 6.226966478309651443, 13.75515049843148674, -1.330623856768273106 ) ) ;
#17709 = DIRECTION ( 'NONE',  ( 1.000000000000000000, 0.000000000000000000, 0.000000000000000000 ) ) ;
#17710 = ADVANCED_FACE ( 'NONE', ( #5185 ), #3707, .T. ) ;
#17711 = AXIS2_PLACEMENT_3D ( 'NONE', #2261, #18735, #2142 ) ;
#17712 = EDGE_LOOP ( 'NONE', ( #16247, #14809, #15376, #2650 ) ) ;
#17713 = EDGE_CURVE ( 'NONE', #8845, #5602, #15828, .T. ) ;
#17714 = FACE_OUTER_BOUND ( 'NONE', #7385, .T. ) ;
#17715 = CARTESIAN_POINT ( 'NONE',  ( 3.653528746108709147, 24.70780860099632292, 2.509315635922550580 ) ) ;
#17716 = DIRECTION ( 'NONE',  ( 0.000000000000000000, 0.000000000000000000, -1.000000000000000000 ) ) ;
#17717 = ORIENTED_EDGE ( 'NONE', *, *, #3051, .T. ) ;
#17718 = CARTESIAN_POINT ( 'NONE',  ( -24.10441230706999960, 7.126933907174000105, -8.778685816131000408 ) ) ;
#17719 = CARTESIAN_POINT ( 'NONE',  ( 2.818367767609802677, 28.05137445130671381, -2.991616928423186828 ) ) ;
#17720 = DIRECTION ( 'NONE',  ( 1.000000000000000000, 0.000000000000000000, 0.000000000000000000 ) ) ;
#17721 = CARTESIAN_POINT ( 'NONE',  ( 15.23247813278353746, 4.705309158913490108, 9.205882947448541742 ) ) ;
#17722 = CARTESIAN_POINT ( 'NONE',  ( 11.77156519342000074, 1.080486702797000030E-14, 0.000000000000000000 ) ) ;
#17723 = LINE ( 'NONE', #20984, #12255 ) ;
#17724 = DIRECTION ( 'NONE',  ( 0.000000000000000000, 1.000000000000000000, 0.000000000000000000 ) ) ;
#17725 = CARTESIAN_POINT ( 'NONE',  ( -3.895265127482998579, 12.15836816443999702, -2.782973809895999295 ) ) ;
#17726 = EDGE_LOOP ( 'NONE', ( #10794, #1824, #1971, #15887 ) ) ;
#17727 = CIRCLE ( 'NONE', #21969, 0.5500000000000001554 ) ;
#17728 = CARTESIAN_POINT ( 'NONE',  ( -1.957297221654172192, 29.45966400265699292, 0.9176472163504577617 ) ) ;
#17729 = ORIENTED_EDGE ( 'NONE', *, *, #22848, .F. ) ;
#17730 = B_SPLINE_CURVE_WITH_KNOTS ( 'NONE', 3,
 ( #13573, #20967, #11767, #9942 ),
 .UNSPECIFIED., .F., .F.,
 ( 4, 4 ),
 ( 0.000000000000000000, 1.000000000000000000 ),
 .UNSPECIFIED. ) ;
#17731 = CARTESIAN_POINT ( 'NONE',  ( -0.5723425338777000659, 23.45465430019000053, -2.197853533198000253 ) ) ;
#17732 = CARTESIAN_POINT ( 'NONE',  ( -16.63345270903459294, 9.745656342660240057, 3.687025462406674503 ) ) ;
#17733 = EDGE_LOOP ( 'NONE', ( #22310, #2756, #3871 ) ) ;
#17734 = AXIS2_PLACEMENT_3D ( 'NONE', #22877, #17446, #1090 ) ;
#17735 = CARTESIAN_POINT ( 'NONE',  ( 6.372376369063001533, 13.56112563602000165, -1.886254648120999411 ) ) ;
#17736 = CARTESIAN_POINT ( 'NONE',  ( 11.99999999999999822, 1.399482473622788659, -8.879313528662020616 ) ) ;
#17737 = CARTESIAN_POINT ( 'NONE',  ( -19.95647087121332675, 1.202231731695357908, -9.183404087729607923 ) ) ;
#17738 = CARTESIAN_POINT ( 'NONE',  ( 16.38112658530999610, 10.11489150981000051, 1.477102707085000022 ) ) ;
#17739 = EDGE_CURVE ( 'NONE', #7057, #23948, #5416, .T. ) ;
#17740 = ORIENTED_EDGE ( 'NONE', *, *, #8687, .T. ) ;
#17741 = DIRECTION ( 'NONE',  ( -0.7071067811865975328, 0.000000000000000000, 0.7071067811864976127 ) ) ;
#17742 = AXIS2_PLACEMENT_3D ( 'NONE', #17702, #8134, #14058 ) ;
#17743 = CARTESIAN_POINT ( 'NONE',  ( -0.6836813991252411737, 24.62756664670458662, -4.224074002601207134 ) ) ;
#17744 = CARTESIAN_POINT ( 'NONE',  ( -20.44776253787999920, -9.196011600180998613, 0.000000000000000000 ) ) ;
#17745 = ORIENTED_EDGE ( 'NONE', *, *, #10839, .F. ) ;
#17746 = CARTESIAN_POINT ( 'NONE',  ( 11.83261479513476999, 13.04738324256021897, 2.401298039133532125 ) ) ;
#17747 = CARTESIAN_POINT ( 'NONE',  ( 0.000000000000000000, 15.00000000000000000, 0.000000000000000000 ) ) ;
#17748 = CARTESIAN_POINT ( 'NONE',  ( -5.819905644321182514, 14.78666136312912549, -4.230997804075329327 ) ) ;
#17749 = CARTESIAN_POINT ( 'NONE',  ( 16.21516467252304494, -2.163961224650327253, -10.13852251010399641 ) ) ;
#17750 = B_SPLINE_CURVE_WITH_KNOTS ( 'NONE', 3,
 ( #23039, #6459, #3206, #10099, #10588, #13843, #17612, #1005 ),
 .UNSPECIFIED., .F., .F.,
 ( 4, 2, 2, 4 ),
 ( 0.000000000000000000, 0.2499999999999990563, 0.4999999999999981126, 1.000000000000000000 ),
 .UNSPECIFIED. ) ;
#17751 = CARTESIAN_POINT ( 'NONE',  ( -23.74465998031000069, 7.716878364870000340, 11.63397459621999985 ) ) ;
#17752 = DIRECTION ( 'NONE',  ( -1.000000000000000000, 0.000000000000000000, 0.000000000000000000 ) ) ;
#17753 = AXIS2_PLACEMENT_3D ( 'NONE', #4709, #12094, #8696 ) ;
#17754 = CARTESIAN_POINT ( 'NONE',  ( -4.281325311130067313, 13.62243467556385212, -4.949493687103234230 ) ) ;
#17755 = LINE ( 'NONE', #8663, #1041 ) ;
#17756 = CARTESIAN_POINT ( 'NONE',  ( -1.422584979458079157, 30.09537825555706547, -1.627545391958989507 ) ) ;
#17757 = ORIENTED_EDGE ( 'NONE', *, *, #12143, .T. ) ;
#17758 = CARTESIAN_POINT ( 'NONE',  ( 2.230746854092000131, 25.83406370960000231, -0.3522458802031000480 ) ) ;
#17759 = CARTESIAN_POINT ( 'NONE',  ( 23.37160127288000311, 7.821747501224999510, -7.657236109244999867 ) ) ;
#17760 = CARTESIAN_POINT ( 'NONE',  ( -12.25000000000000000, 1.374666032043000015E-14, 0.000000000000000000 ) ) ;
#17761 = CARTESIAN_POINT ( 'NONE',  ( 0.000000000000000000, 28.00000000000000000, 0.000000000000000000 ) ) ;
#17762 = ORIENTED_EDGE ( 'NONE', *, *, #5783, .F. ) ;
#17763 = CARTESIAN_POINT ( 'NONE',  ( -19.35893705290999733, -9.828989445528000246, 3.502754984265999738 ) ) ;
#17764 = CARTESIAN_POINT ( 'NONE',  ( -24.50000000000292744, -10.95355345393464574, -6.027888894374386908 ) ) ;
#17765 = CARTESIAN_POINT ( 'NONE',  ( -4.946046029160003243, 12.51485534603999383, -0.01135644941591000372 ) ) ;
#17766 = ORIENTED_EDGE ( 'NONE', *, *, #23886, .F. ) ;
#17767 = AXIS2_PLACEMENT_3D ( 'NONE', #22138, #14514, #1917 ) ;
#17768 = CARTESIAN_POINT ( 'NONE',  ( -16.40044400686480586, 9.230068319053810200, 4.808581141419865368 ) ) ;
#17769 = CARTESIAN_POINT ( 'NONE',  ( 17.09606375731000227, -3.490954664894000192, -8.536518206589999380 ) ) ;
#17770 = VERTEX_POINT ( 'NONE', #12801 ) ;
#17771 = AXIS2_PLACEMENT_3D ( 'NONE', #19354, #2881, #22962 ) ;
#17772 = CARTESIAN_POINT ( 'NONE',  ( 1.486729910992351078, 27.12575827504875647, 1.582850948029659088 ) ) ;
#17773 = CARTESIAN_POINT ( 'NONE',  ( 0.000000000000000000, 0.000000000000000000, 0.000000000000000000 ) ) ;
#17774 = LINE ( 'NONE', #6501, #20644 ) ;
#17775 = ORIENTED_EDGE ( 'NONE', *, *, #14592, .F. ) ;
#17776 = CARTESIAN_POINT ( 'NONE',  ( -4.000000000000000000, 28.30000000000000071, 2.309401076759000304 ) ) ;
#17777 = VECTOR ( 'NONE', #17575, 1000.000000000000000 ) ;
#17778 = CARTESIAN_POINT ( 'NONE',  ( -4.547121837679138245, 15.52640757196256338, -4.103591966345952358 ) ) ;
#17779 = CARTESIAN_POINT ( 'NONE',  ( -22.45307115331999981, 4.633966765693999790, -10.17689589833000063 ) ) ;
#17780 = EDGE_CURVE ( 'NONE', #3196, #1114, #3842, .T. ) ;
#17781 = CARTESIAN_POINT ( 'NONE',  ( -19.96098122809999964, -10.36515734744000028, 0.7445752835680999882 ) ) ;
#17782 = CARTESIAN_POINT ( 'NONE',  ( 0.3480762113532999691, 27.25000000000000000, -6.000000000000000000 ) ) ;
#17783 = CARTESIAN_POINT ( 'NONE',  ( 18.23994494525999954, -9.523641201324000605, -4.050084129495000518 ) ) ;
#17784 = CARTESIAN_POINT ( 'NONE',  ( 4.829987487923999900, 14.79876397742000016, -3.766541047082999860 ) ) ;
#17785 = CARTESIAN_POINT ( 'NONE',  ( 20.58441673460000132, -2.591490884510000203, -9.327754992274998713 ) ) ;
#17786 = CIRCLE ( 'NONE', #10049, 4.000000000000000000 ) ;
#17787 = CARTESIAN_POINT ( 'NONE',  ( 24.50000000000000000, 8.054858440593999802, 5.882793087032000656 ) ) ;
#17788 = ORIENTED_EDGE ( 'NONE', *, *, #18144, .F. ) ;
#17789 = CARTESIAN_POINT ( 'NONE',  ( 23.65010203509851294, -1.257950004970036506, 9.261471990918924035 ) ) ;
#17790 = CARTESIAN_POINT ( 'NONE',  ( 2.815613996704550370, 14.07709565253041362, 5.439481458778258727 ) ) ;
#17791 = CARTESIAN_POINT ( 'NONE',  ( -0.5724186824819998964, 25.97619850838000133, -2.193530619437999984 ) ) ;
#17792 = VECTOR ( 'NONE', #4744, 1000.000000000000000 ) ;
#17793 = CIRCLE ( 'NONE', #11591, 7.000000000000000000 ) ;
#17794 = CYLINDRICAL_SURFACE ( 'NONE', #16954, 7.100000000000000533 ) ;
#17795 = CARTESIAN_POINT ( 'NONE',  ( -14.17283651172096981, 8.841951170099118684, -2.221021055535443267 ) ) ;
#17796 = ADVANCED_FACE ( 'NONE', ( #7103 ), #20188, .T. ) ;
#17797 = CARTESIAN_POINT ( 'NONE',  ( 1.008585698963999855, 28.87437716036000168, 1.979460888490000015 ) ) ;
#17798 = CARTESIAN_POINT ( 'NONE',  ( -4.630910936227792263, 12.36731740134543323, 1.448661297286960803 ) ) ;
#17799 = ORIENTED_EDGE ( 'NONE', *, *, #10145, .T. ) ;
#17800 = CARTESIAN_POINT ( 'NONE',  ( 1.399999999999999911, 7.000000000000000000, 0.000000000000000000 ) ) ;
#17801 = CARTESIAN_POINT ( 'NONE',  ( 1.541259979151140769, 11.58204529230899915, -4.568150535643495047 ) ) ;
#17802 = DIRECTION ( 'NONE',  ( 0.000000000000000000, 1.000000000000000000, 0.000000000000000000 ) ) ;
#17803 = CARTESIAN_POINT ( 'NONE',  ( -21.09022087121333300, 5.661420876518568512, 7.367019229478493969 ) ) ;
#17804 = CARTESIAN_POINT ( 'NONE',  ( 11.50000000000000000, 0.000000000000000000, 0.000000000000000000 ) ) ;
#17805 = CARTESIAN_POINT ( 'NONE',  ( -2.197444295422539717, 30.81144470851556960, -0.03941198171681850604 ) ) ;
#17806 = CARTESIAN_POINT ( 'NONE',  ( -2.500000000000000000, 29.83419673618999823, 0.000000000000000000 ) ) ;
#17807 = CARTESIAN_POINT ( 'NONE',  ( 18.51187642130999933, -4.805399430337999434, 8.325799818148999165 ) ) ;
#17808 = CARTESIAN_POINT ( 'NONE',  ( -2.434931691670787934, 27.23333333333334139, 0.6543697108982051702 ) ) ;
#17809 = EDGE_CURVE ( 'NONE', #20876, #8805, #11589, .T. ) ;
#17810 = ORIENTED_EDGE ( 'NONE', *, *, #16225, .F. ) ;
#17811 = CARTESIAN_POINT ( 'NONE',  ( -2.184465970885646424, 28.73333333333333428, -1.259047450927245126 ) ) ;
#17812 = CARTESIAN_POINT ( 'NONE',  ( 0.8513612441708000578, 29.31092011053999968, -2.385437969772000066 ) ) ;
#17813 = CARTESIAN_POINT ( 'NONE',  ( -15.12503743917333487, -1.186002250417325099, 9.059419983607615023 ) ) ;
#17814 = CARTESIAN_POINT ( 'NONE',  ( -2.491868457724357722, 13.99434024406236787, -5.595226495223592167 ) ) ;
#17815 = AXIS2_PLACEMENT_3D ( 'NONE', #7449, #13147, #16890 ) ;
#17816 = ORIENTED_EDGE ( 'NONE', *, *, #21535, .T. ) ;
#17817 = LINE ( 'NONE', #5214, #5984 ) ;
#17818 = CARTESIAN_POINT ( 'NONE',  ( 24.49181240879000043, -4.016481066597000549, 10.13876987169999921 ) ) ;
#17819 = FACE_OUTER_BOUND ( 'NONE', #9376, .T. ) ;
#17820 = PLANE ( 'NONE',  #2296 ) ;
#17821 = CARTESIAN_POINT ( 'NONE',  ( 15.78600699156848819, -8.833878469997333838, -5.484853103214551773 ) ) ;
#17822 = CARTESIAN_POINT ( 'NONE',  ( -3.839124943223277242, 14.03390693797235755, 4.849677718342541688 ) ) ;
#17823 = CARTESIAN_POINT ( 'NONE',  ( -21.81416243917332665, -8.065940078106184075, -4.649062424942554728 ) ) ;
#17824 = ADVANCED_FACE ( 'NONE', ( #12567 ), #4374, .F. ) ;
#17825 = CARTESIAN_POINT ( 'NONE',  ( -2.750000000000000000, 24.29999999999999716, 0.000000000000000000 ) ) ;
#17826 = ORIENTED_EDGE ( 'NONE', *, *, #14448, .T. ) ;
#17827 = DIRECTION ( 'NONE',  ( 0.000000000000000000, 0.000000000000000000, 1.000000000000000000 ) ) ;
#17828 = CARTESIAN_POINT ( 'NONE',  ( 11.18529249867181363, -11.69879683431631179, 4.737131156288532985 ) ) ;
#17829 = ORIENTED_EDGE ( 'NONE', *, *, #14709, .F. ) ;
#17830 = CARTESIAN_POINT ( 'NONE',  ( -0.6940159635513000191, 23.79121626938999867, -2.361381702958999629 ) ) ;
#17831 = DIRECTION ( 'NONE',  ( 1.000000000000000000, 0.000000000000000000, 0.000000000000000000 ) ) ;
#17832 = CARTESIAN_POINT ( 'NONE',  ( -0.4485994107868310210, 12.81051815475211519, 6.650126618851852633 ) ) ;
#17833 = CARTESIAN_POINT ( 'NONE',  ( 6.233555060839315765, 13.72084049725845567, -1.474633800018174679 ) ) ;
#17834 = CARTESIAN_POINT ( 'NONE',  ( -5.983874849942004026, 15.83682689383999076, -0.8929930702161996692 ) ) ;
#17835 = EDGE_CURVE ( 'NONE', #20342, #5650, #10808, .T. ) ;
#17836 = DIRECTION ( 'NONE',  ( 0.000000000000000000, 0.000000000000000000, -1.000000000000000000 ) ) ;
#17837 = ORIENTED_EDGE ( 'NONE', *, *, #18558, .T. ) ;
#17838 = CARTESIAN_POINT ( 'NONE',  ( -12.30391311677716359, 12.15793044322834504, -9.412942108898313620 ) ) ;
#17839 = CARTESIAN_POINT ( 'NONE',  ( -1.937289889703149859, 26.22758819317520818, 0.8800478335377882599 ) ) ;
#17840 = LINE ( 'NONE', #6678, #12893 ) ;
#17841 = EDGE_CURVE ( 'NONE', #5021, #6219, #5643, .T. ) ;
#17842 = ORIENTED_EDGE ( 'NONE', *, *, #8643, .F. ) ;
#17843 = CARTESIAN_POINT ( 'NONE',  ( -23.68915714226000091, 10.30687545221999990, -3.135322633623999877 ) ) ;
#17844 = EDGE_CURVE ( 'NONE', #4978, #16650, #15377, .T. ) ;
#17845 = CARTESIAN_POINT ( 'NONE',  ( 20.30216666666665759, -8.032133636156673973, -4.629287041203744124 ) ) ;
#17846 = CARTESIAN_POINT ( 'NONE',  ( 15.15146838647111238, 7.118369732183343679, 7.496456199561704281 ) ) ;
#17847 = CARTESIAN_POINT ( 'NONE',  ( 3.999996093285163035, 24.62756664670878948, 1.519951541579177778 ) ) ;
#17848 = DIRECTION ( 'NONE',  ( -1.000000000000000000, 0.000000000000000000, 0.000000000000000000 ) ) ;
#17849 = CARTESIAN_POINT ( 'NONE',  ( 13.59924040960673786, 6.893992233393349878, -5.816697367115062356 ) ) ;
#17850 = CARTESIAN_POINT ( 'NONE',  ( -3.149587440023998486, 12.07849849174000312, -3.556593144048001864 ) ) ;
#17851 = ORIENTED_EDGE ( 'NONE', *, *, #14592, .T. ) ;
#17852 = FACE_OUTER_BOUND ( 'NONE', #3818, .T. ) ;
#17853 = CARTESIAN_POINT ( 'NONE',  ( -2.009380400686512580, 29.45175883193518374, 0.7931520617424835384 ) ) ;
#17854 = EDGE_CURVE ( 'NONE', #7466, #14519, #16897, .T. ) ;
#17855 = EDGE_LOOP ( 'NONE', ( #16879, #12590, #11450, #23127 ) ) ;
#17856 = DIRECTION ( 'NONE',  ( -1.000000000000000000, 0.000000000000000000, 0.000000000000000000 ) ) ;
#17857 = CARTESIAN_POINT ( 'NONE',  ( -17.58844544603152116, -10.40508157927476951, -2.008783379089892573 ) ) ;
#17858 = ORIENTED_EDGE ( 'NONE', *, *, #1393, .F. ) ;
#17859 = CARTESIAN_POINT ( 'NONE',  ( 4.924532323579002835, 14.11581327235000316, -3.892461550489000111 ) ) ;
#17860 = CARTESIAN_POINT ( 'NONE',  ( 12.00000000000000000, 2.690641297232414519, -8.571655010542230002 ) ) ;
#17861 = CARTESIAN_POINT ( 'NONE',  ( 18.66303164209000087, 0.6515539281180999787, 11.11005403933000046 ) ) ;
#17862 = CARTESIAN_POINT ( 'NONE',  ( 18.93037674931000325, -2.874963284959999754, 10.40852167983000065 ) ) ;
#17863 = ORIENTED_EDGE ( 'NONE', *, *, #20932, .T. ) ;
#17864 = CARTESIAN_POINT ( 'NONE',  ( -10.52007399291999867, -1.707568499793000072, -14.41682586501999985 ) ) ;
#17865 = DIRECTION ( 'NONE',  ( 0.000000000000000000, 1.000000000000000000, 0.000000000000000000 ) ) ;
#17866 = DIRECTION ( 'NONE',  ( 0.1709999999999925469, 0.9852710287022563573, 0.000000000000000000 ) ) ;
#17867 = EDGE_CURVE ( 'NONE', #12256, #3010, #13936, .T. ) ;
#17868 = ORIENTED_EDGE ( 'NONE', *, *, #9343, .T. ) ;
#17869 = EDGE_CURVE ( 'NONE', #4443, #10646, #21644, .T. ) ;
#17870 = DIRECTION ( 'NONE',  ( 0.000000000000000000, 0.000000000000000000, -1.000000000000000000 ) ) ;
#17871 = CARTESIAN_POINT ( 'NONE',  ( 22.32342665428159378, 3.749095308366488410, 9.883727313549222515 ) ) ;
#17872 = CARTESIAN_POINT ( 'NONE',  ( -6.249999999916000526, 15.09564573669999987, 3.212813967733000098 ) ) ;
#17873 = CARTESIAN_POINT ( 'NONE',  ( 16.33715996058963427, 2.151044717592483835, -10.15474803909974000 ) ) ;
#17874 = CARTESIAN_POINT ( 'NONE',  ( -5.758336963890107185, 14.73197845513246662, 4.351221581719583398 ) ) ;
#17875 = CARTESIAN_POINT ( 'NONE',  ( -14.48092000065305385, -9.982182315257093208, 7.710362946285843400 ) ) ;
#17876 = CARTESIAN_POINT ( 'NONE',  ( 1.182434930542718865, 26.44682129341587284, 3.936123028068912344 ) ) ;
#17877 = CARTESIAN_POINT ( 'NONE',  ( -1.904442799929577879, 30.26744504660184631, 1.036340829782300688 ) ) ;
#17878 = EDGE_CURVE ( 'NONE', #10966, #14748, #9273, .T. ) ;
#17879 = ORIENTED_EDGE ( 'NONE', *, *, #15103, .T. ) ;
#17880 = CARTESIAN_POINT ( 'NONE',  ( 11.40904387244416185, 9.351110459849435230, -8.803306989966603879 ) ) ;
#17881 = EDGE_CURVE ( 'NONE', #14333, #3210, #8762, .T. ) ;
#17882 = CARTESIAN_POINT ( 'NONE',  ( 22.65423997573916992, -1.018721363148856529, 10.53549965532916133 ) ) ;
#17883 = CARTESIAN_POINT ( 'NONE',  ( 60.61494135913342518, 35.51856778792605240, -2.673746900119611247 ) ) ;
#17884 = VERTEX_POINT ( 'NONE', #5163 ) ;
#17885 =( BOUNDED_CURVE ( )  B_SPLINE_CURVE ( 3, ( #17872, #5040, #10604, #19922 ),
 .UNSPECIFIED., .F., .T. ) 
 B_SPLINE_CURVE_WITH_KNOTS ( ( 4, 4 ),
 ( 0.000000000000000000, 1.000000000000000000 ),
 .UNSPECIFIED. ) 
 CURVE ( )  GEOMETRIC_REPRESENTATION_ITEM ( )  RATIONAL_B_SPLINE_CURVE ( ( 1.134253127167035746, 0.9460051651271520479, 0.9557263079415558860, 1.163416555610247594 ) ) 
 REPRESENTATION_ITEM ( '' )  );
#17886 = CARTESIAN_POINT ( 'NONE',  ( 24.50000000000000355, -10.31403833462485053, -7.135561573215231768 ) ) ;
#17887 = FACE_OUTER_BOUND ( 'NONE', #17407, .T. ) ;
#17888 = ORIENTED_EDGE ( 'NONE', *, *, #4812, .F. ) ;
#17889 = CARTESIAN_POINT ( 'NONE',  ( -15.06070461986450049, 4.116752997674038461, -9.515275712647939699 ) ) ;
#17890 = DIRECTION ( 'NONE',  ( -1.000000000000000000, 0.000000000000000000, 0.000000000000000000 ) ) ;
#17891 = ORIENTED_EDGE ( 'NONE', *, *, #16173, .F. ) ;
#17892 = LINE ( 'NONE', #1042, #932 ) ;
#17893 = SHAPE_DEFINITION_REPRESENTATION ( #19268, #13682 ) ;
#17894 = DIRECTION ( 'NONE',  ( 0.000000000000000000, 0.7941276157285981352, 0.6077510427281981320 ) ) ;
#17895 = VERTEX_POINT ( 'NONE', #4921 ) ;
#17896 = CARTESIAN_POINT ( 'NONE',  ( 2.500000000000003109, 26.77499936725412866, 0.4908862760595652519 ) ) ;
#17897 = CARTESIAN_POINT ( 'NONE',  ( 12.78787674931000140, 8.861872729009999006, -5.882981327196000088 ) ) ;
#17898 = CARTESIAN_POINT ( 'NONE',  ( -22.72225193867999948, 4.421850665685999715, -9.710967849992998779 ) ) ;
#17899 = CARTESIAN_POINT ( 'NONE',  ( -15.42606313537000062, 5.797595928499999829, -9.114297677153000876 ) ) ;
#17900 = CARTESIAN_POINT ( 'NONE',  ( 22.34291666666665321, -2.419883552198663690, -9.003983045265712803 ) ) ;
#17901 = CARTESIAN_POINT ( 'NONE',  ( 18.30812451746000136, -9.368717106552999496, 2.913269227472000011 ) ) ;
#17902 = CARTESIAN_POINT ( 'NONE',  ( -2.132962310478440315, 27.02892739381266907, 0.4133339932766221803 ) ) ;
#17903 = CARTESIAN_POINT ( 'NONE',  ( 13.65000000000000036, 1.057482511063999969E-14, 0.000000000000000000 ) ) ;
#17904 = CARTESIAN_POINT ( 'NONE',  ( 24.46338342271116062, 9.116595994419974147, 4.069120185925712008 ) ) ;
#17905 = VERTEX_POINT ( 'NONE', #12070 ) ;
#17906 = CARTESIAN_POINT ( 'NONE',  ( 23.35066019142154659, 7.280967731064075465, 5.766833715589692488 ) ) ;
#17907 = CARTESIAN_POINT ( 'NONE',  ( 0.1555892161840528309, 13.69209904246603493, 6.123026241355283616 ) ) ;
#17908 = CARTESIAN_POINT ( 'NONE',  ( -2.263084017374999757, 26.95119850837999920, 0.1334610483750000021 ) ) ;
#17909 = AXIS2_PLACEMENT_3D ( 'NONE', #10080, #4386, #19404 ) ;
#17910 = DIRECTION ( 'NONE',  ( 0.000000000000000000, 1.000000000000000000, 0.000000000000000000 ) ) ;
#17911 = CARTESIAN_POINT ( 'NONE',  ( 6.015441748752945017, 14.40198550462790017, -1.164718804201562818 ) ) ;
#17912 = CARTESIAN_POINT ( 'NONE',  ( -21.91519891963999811, 2.578799165454999986, 10.79911247067000168 ) ) ;
#17913 = CARTESIAN_POINT ( 'NONE',  ( -3.374921343011017871, 11.96071138814094859, 3.456569768525166175 ) ) ;
#17914 = ORIENTED_EDGE ( 'NONE', *, *, #11499, .T. ) ;
#17915 = CARTESIAN_POINT ( 'NONE',  ( 15.74912270046332274, 7.929943201579005674, -4.570678727046721512 ) ) ;
#17916 = CARTESIAN_POINT ( 'NONE',  ( 3.972980349958184831, 12.14025353368746174, -2.760264024277557571 ) ) ;
#17917 = CARTESIAN_POINT ( 'NONE',  ( -10.62890643558121617, 15.45176336733469036, 1.489320882496812493 ) ) ;
#17918 = CARTESIAN_POINT ( 'NONE',  ( 11.95587595596410679, 4.161512325801380641, -8.073311510776072453 ) ) ;
#17919 = ORIENTED_EDGE ( 'NONE', *, *, #13696, .F. ) ;
#17920 = CARTESIAN_POINT ( 'NONE',  ( -1.869327042239785852, 30.61308158997630002, -1.502106005567143354 ) ) ;
#17921 = CARTESIAN_POINT ( 'NONE',  ( -13.10414243475000085, 9.447148007457000674, -4.942668164112999918 ) ) ;
#17922 = CARTESIAN_POINT ( 'NONE',  ( 16.68375142130999933, -4.435783964195000095, 8.649968580473998969 ) ) ;
#17923 = CARTESIAN_POINT ( 'NONE',  ( 18.51005996110214014, 10.35102410635204606, -1.233439651704276274 ) ) ;
#17924 = VERTEX_POINT ( 'NONE', #6843 ) ;
#17925 = CARTESIAN_POINT ( 'NONE',  ( 0.000000000000000000, 17.00000000000000000, -4.649999999999999467 ) ) ;
#17926 = CARTESIAN_POINT ( 'NONE',  ( -1.625358910797000123, 29.44327955148999720, -1.942508336889000153 ) ) ;
#17927 = CARTESIAN_POINT ( 'NONE',  ( -11.00000000000000000, 1.359357947053999856E-14, 0.000000000000000000 ) ) ;
#17928 = CARTESIAN_POINT ( 'NONE',  ( 3.187263766028701539, 14.18382903446076249, -5.230654009935672200 ) ) ;
#17929 = ORIENTED_EDGE ( 'NONE', *, *, #11940, .T. ) ;
#17930 = DIRECTION ( 'NONE',  ( 0.000000000000000000, 1.000000000000000000, 0.000000000000000000 ) ) ;
#17931 = DIRECTION ( 'NONE',  ( 0.000000000000000000, 1.000000000000000000, 0.000000000000000000 ) ) ;
#17932 = DIRECTION ( 'NONE',  ( -1.000000000000000000, 0.000000000000000000, 0.000000000000000000 ) ) ;
#17933 = CARTESIAN_POINT ( 'NONE',  ( -12.50000000000000000, 6.992973968623999781, -5.709239639804999378 ) ) ;
#17934 = CARTESIAN_POINT ( 'NONE',  ( 14.39214709631707834, 4.421562029032312324, -9.372419967397966900 ) ) ;
#17935 = DIRECTION ( 'NONE',  ( -1.000000000000000000, 0.000000000000000000, 0.000000000000000000 ) ) ;
#17936 = CARTESIAN_POINT ( 'NONE',  ( 4.902363039930995647, 12.49825868767001147, 0.6843989955805002134 ) ) ;
#17937 = DIRECTION ( 'NONE',  ( 1.000000000000000000, 0.000000000000000000, 0.000000000000000000 ) ) ;
#17938 = ORIENTED_EDGE ( 'NONE', *, *, #4899, .T. ) ;
#17939 = DIRECTION ( 'NONE',  ( 0.000000000000000000, 0.000000000000000000, -1.000000000000000000 ) ) ;
#17940 =( GEOMETRIC_REPRESENTATION_CONTEXT ( 3 ) GLOBAL_UNCERTAINTY_ASSIGNED_CONTEXT ( ( #12539 ) ) GLOBAL_UNIT_ASSIGNED_CONTEXT ( ( #21285, #19712, #8199 ) ) REPRESENTATION_CONTEXT ( 'NONE', 'WORKASPACE' ) );
#17941 = CARTESIAN_POINT ( 'NONE',  ( 2.000000000000198508, 24.49999999999999645, -3.464101615138341028 ) ) ;
#17942 = ORIENTED_EDGE ( 'NONE', *, *, #9381, .T. ) ;
#17943 = EDGE_CURVE ( 'NONE', #19018, #12884, #12235, .T. ) ;
#17944 = DIRECTION ( 'NONE',  ( 0.000000000000000000, 1.000000000000000000, 0.000000000000000000 ) ) ;
#17945 = CARTESIAN_POINT ( 'NONE',  ( 11.10357421856130600, -0.9986522863917048909, -12.49997040256712388 ) ) ;
#17946 = VECTOR ( 'NONE', #7805, 1000.000000000000114 ) ;
#17947 = CARTESIAN_POINT ( 'NONE',  ( 6.179202422571329123, 13.97195698268568087, -0.6507670915169003756 ) ) ;
#17948 = CARTESIAN_POINT ( 'NONE',  ( 13.49999999999999822, 0.5660735980287910918, 10.31195207906871403 ) ) ;
#17949 = DIRECTION ( 'NONE',  ( 0.9771428571428639742, 0.000000000000000000, 0.2125837170026919909 ) ) ;
#17950 = ORIENTED_EDGE ( 'NONE', *, *, #20523, .T. ) ;
#17951 = CARTESIAN_POINT ( 'NONE',  ( -3.268181200173220002, 29.87490599056235041, -2.731916857836431234 ) ) ;
#17952 = CARTESIAN_POINT ( 'NONE',  ( 0.000000000000000000, 17.89999999999999858, -3.000000000002987832 ) ) ;
#17953 = APPLICATION_CONTEXT ( 'automotive_design' ) ;
#17954 = CARTESIAN_POINT ( 'NONE',  ( -1.399999999999999911, 7.000000000000000000, 0.000000000000000000 ) ) ;
#17955 = ORIENTED_EDGE ( 'NONE', *, *, #1841, .T. ) ;
#17956 = EDGE_CURVE ( 'NONE', #10339, #9862, #10186, .T. ) ;
#17957 = CARTESIAN_POINT ( 'NONE',  ( -24.03189061347999811, 0.9515185275740000170, -10.74041837823999934 ) ) ;
#17958 = DIRECTION ( 'NONE',  ( -0.4226182617406808451, 0.000000000000000000, 0.9063077870366587074 ) ) ;
#17959 = CARTESIAN_POINT ( 'NONE',  ( 15.06085725605862358, 9.069360526526905275, 4.955433154737670876 ) ) ;
#17960 = AXIS2_PLACEMENT_3D ( 'NONE', #17460, #17709, #1106 ) ;
#17961 = DIRECTION ( 'NONE',  ( -1.000000000000000000, 0.000000000000000000, 0.000000000000000000 ) ) ;
#17962 = CARTESIAN_POINT ( 'NONE',  ( 2.045270984003000336, 28.93354368677000110, -0.7190670843306999904 ) ) ;
#17963 = CARTESIAN_POINT ( 'NONE',  ( 1.699986222664000124, 9.100024384209000061, 1.053575639828000066 ) ) ;
#17964 = CARTESIAN_POINT ( 'NONE',  ( -4.782017827913002783, 12.48036279474998977, -0.01094907448527000608 ) ) ;
#17965 = EDGE_LOOP ( 'NONE', ( #15912, #15772, #3720, #18106 ) ) ;
#17966 = CARTESIAN_POINT ( 'NONE',  ( -21.88384587121331393, -2.416565420321704849, -8.992606164485385634 ) ) ;
#17967 = ORIENTED_EDGE ( 'NONE', *, *, #23738, .F. ) ;
#17968 = AXIS2_PLACEMENT_3D ( 'NONE', #16246, #21711, #18075 ) ;
#17969 = AXIS2_PLACEMENT_3D ( 'NONE', #18010, #1294, #21760 ) ;
#17970 = DIRECTION ( 'NONE',  ( 0.000000000000000000, -1.000000000000000000, 0.000000000000000000 ) ) ;
#17971 = CARTESIAN_POINT ( 'NONE',  ( 2.999999956181000016, 17.90000004382000043, -2.609181548331000199E-08 ) ) ;
#17972 = VERTEX_POINT ( 'NONE', #271 ) ;
#17973 = EDGE_CURVE ( 'NONE', #19300, #11498, #12129, .T. ) ;
#17974 = CARTESIAN_POINT ( 'NONE',  ( -1.584557413972607076, 30.28301061182800780, -2.080722500251575457 ) ) ;
#17975 = CARTESIAN_POINT ( 'NONE',  ( 12.06371966924003658, -13.38412994814091306, -1.818205398009610008 ) ) ;
#17976 = LINE ( 'NONE', #2958, #19699 ) ;
#17977 = CARTESIAN_POINT ( 'NONE',  ( 16.67807176579999862, 6.709682755504000617, 8.811495003121999403 ) ) ;
#17978 = CARTESIAN_POINT ( 'NONE',  ( 1.745401010056999880, 27.08506359724000134, 1.745401010056999880 ) ) ;
#17979 = CARTESIAN_POINT ( 'NONE',  ( 18.82068924930999998, 1.189837805593999986, 10.72966125727000097 ) ) ;
#17980 = ORIENTED_EDGE ( 'NONE', *, *, #20589, .F. ) ;
#17981 = CARTESIAN_POINT ( 'NONE',  ( -10.92736399291999838, -14.05489928066999994, 3.635995652016000168 ) ) ;
#17982 = CARTESIAN_POINT ( 'NONE',  ( 13.49999999999999822, 8.021967196418742674, -4.687592336913057878 ) ) ;
#17983 = DIRECTION ( 'NONE',  ( 0.000000000000000000, -1.000000000000000000, 0.000000000000000000 ) ) ;
#17984 = ORIENTED_EDGE ( 'NONE', *, *, #17713, .T. ) ;
#17985 = EDGE_CURVE ( 'NONE', #9372, #22807, #20632, .T. ) ;
#17986 = CARTESIAN_POINT ( 'NONE',  ( 0.000000000000000000, 9.000000000000000000, 0.000000000000000000 ) ) ;
#17987 = CARTESIAN_POINT ( 'NONE',  ( 23.41176634503839082, 2.789004178826171465, -10.22545939124784375 ) ) ;
#17988 = B_SPLINE_CURVE_WITH_KNOTS ( 'NONE', 3,
 ( #15057, #5974, #14816, #9380, #13134, #13245, #18817, #20639, #3933, #15287, #2224, #16752, #22680 ),
 .UNSPECIFIED., .F., .F.,
 ( 4, 1, 1, 1, 1, 1, 2, 2, 4 ),
 ( 0.000000000000000000, 0.2500000000000000000, 0.3750000000000000000, 0.4374999999999999445, 0.4687500000000000000, 0.4843750000000000555, 0.4921875000000000000, 0.4999999999999999445, 1.000000000000000000 ),
 .UNSPECIFIED. ) ;
#17989 = DIRECTION ( 'NONE',  ( 0.000000000000000000, 1.000000000000000000, 0.000000000000000000 ) ) ;
#17990 = CARTESIAN_POINT ( 'NONE',  ( 16.30560488073658831, 1.031953949068942000, -10.32206256363679309 ) ) ;
#17991 = CARTESIAN_POINT ( 'NONE',  ( 0.1765322295559999810, 30.44300150276000139, 2.181163051615000015 ) ) ;
#17992 = VECTOR ( 'NONE', #18188, 1000.000000000000000 ) ;
#17993 = CARTESIAN_POINT ( 'NONE',  ( -3.921362958110083952, 13.93606275262591332, -4.846548280059000291 ) ) ;
#17994 = CARTESIAN_POINT ( 'NONE',  ( 1.461484340634618073, 29.90904337753413955, -1.590560646070451778 ) ) ;
#17995 = VERTEX_POINT ( 'NONE', #397 ) ;
#17996 = CARTESIAN_POINT ( 'NONE',  ( 11.22285964976442862, 11.82554192014311312, -4.517540867263379667 ) ) ;
#17997 = CARTESIAN_POINT ( 'NONE',  ( 23.78917532224939890, 8.220281951958336109, -6.706429737208729591 ) ) ;
#17998 = CARTESIAN_POINT ( 'NONE',  ( -1.269727886480190193, 23.61570448070820305, -1.692922358328529553 ) ) ;
#17999 = VECTOR ( 'NONE', #14899, 1000.000000000000000 ) ;
#18000 = ORIENTED_EDGE ( 'NONE', *, *, #22681, .T. ) ;
#18001 = EDGE_CURVE ( 'NONE', #16978, #12276, #7677, .T. ) ;
#18002 = CARTESIAN_POINT ( 'NONE',  ( -1.908614251018468710, 23.69762311453393977, 1.108721817513677266 ) ) ;
#18003 = DIRECTION ( 'NONE',  ( 0.000000000000000000, 1.000000000000000000, 0.000000000000000000 ) ) ;
#18004 = EDGE_CURVE ( 'NONE', #17545, #1942, #7606, .T. ) ;
#18005 = CARTESIAN_POINT ( 'NONE',  ( -3.150855693194152707, 24.60222989789001957, -2.799640769043123978 ) ) ;
#18006 = EDGE_LOOP ( 'NONE', ( #5092, #12569, #4972, #5854, #4343, #6548, #10544, #863, #22672, #22429, #3280 ) ) ;
#18007 = CARTESIAN_POINT ( 'NONE',  ( 16.65731375730999986, -8.692770150473998925, 3.046645682941000022 ) ) ;
#18008 = VERTEX_POINT ( 'NONE', #5857 ) ;
#18009 = AXIS2_PLACEMENT_3D ( 'NONE', #12965, #3891, #12852 ) ;
#18010 = CARTESIAN_POINT ( 'NONE',  ( -24.50000000000000000, 1.524685264937999788E-14, 0.000000000000000000 ) ) ;
#18011 = PRODUCT_CONTEXT ( 'NONE', #6007, 'mechanical' ) ;
#18012 = CARTESIAN_POINT ( 'NONE',  ( 0.000000000000000000, 7.000000000000000000, 0.000000000000000000 ) ) ;
#18013 = ORIENTED_EDGE ( 'NONE', *, *, #19614, .F. ) ;
#18014 = EDGE_CURVE ( 'NONE', #11394, #6063, #7326, .T. ) ;
#18015 = LINE ( 'NONE', #8815, #11684 ) ;
#18016 = ADVANCED_FACE ( 'NONE', ( #23124 ), #5041, .F. ) ;
#18017 = CARTESIAN_POINT ( 'NONE',  ( -3.900110430061300981, 14.77499599200090152, -4.723055523159343849 ) ) ;
#18018 = CARTESIAN_POINT ( 'NONE',  ( -22.99143272405000360, 4.209734565676999551, -9.245039801656998790 ) ) ;
#18019 = CARTESIAN_POINT ( 'NONE',  ( -14.54251227031000049, -6.905310822002999949, -6.821119646334000031 ) ) ;
#18020 = LINE ( 'NONE', #9043, #16591 ) ;
#18021 = CARTESIAN_POINT ( 'NONE',  ( -23.00635821734891806, -10.16212841000448286, -2.913267094275154179 ) ) ;
#18022 = CARTESIAN_POINT ( 'NONE',  ( -0.2789569746687909357, 27.18793430507837527, 2.190778598715106718 ) ) ;
#18023 = CARTESIAN_POINT ( 'NONE',  ( 2.944270284434495899, 26.42936170367566362, -2.918926912232258530 ) ) ;
#18024 = CARTESIAN_POINT ( 'NONE',  ( 14.78458333333333385, -8.815166781429585541, -2.368879911036435804 ) ) ;
#18025 = ORIENTED_EDGE ( 'NONE', *, *, #3143, .T. ) ;
#18026 = CARTESIAN_POINT ( 'NONE',  ( 1.920340719802868357, 26.32472163128880638, 1.149393952743590130 ) ) ;
#18027 = CARTESIAN_POINT ( 'NONE',  ( -0.6576354733792000307, 28.70619850838000175, 2.169172474974999876 ) ) ;
#18028 = CIRCLE ( 'NONE', #13346, 0.1000000000000002554 ) ;
#18029 = B_SPLINE_CURVE_WITH_KNOTS ( 'NONE', 3,
 ( #6224, #21004, #23176, #13363, #20764 ),
 .UNSPECIFIED., .F., .F.,
 ( 4, 1, 4 ),
 ( 0.000000000000000000, 0.5000000000000000000, 1.000000000000000000 ),
 .UNSPECIFIED. ) ;
#18030 = LINE ( 'NONE', #5424, #5644 ) ;
#18031 = CARTESIAN_POINT ( 'NONE',  ( 2.449054215377000077, 27.41187716035999955, 0.04809324771317000091 ) ) ;
#18032 = CARTESIAN_POINT ( 'NONE',  ( -4.121623016841069465, 12.18874198761142047, 2.540134958274468779 ) ) ;
#18033 = VERTEX_POINT ( 'NONE', #13807 ) ;
#18034 = DIRECTION ( 'NONE',  ( 0.000000000000000000, -1.000000000000000000, 0.000000000000000000 ) ) ;
#18035 = CARTESIAN_POINT ( 'NONE',  ( 2.690147716812516077, 11.78874550216520056, -4.003645878357374066 ) ) ;
#18036 = CARTESIAN_POINT ( 'NONE',  ( 24.17967779705173115, 2.685270347960766024, -9.197338196224221107 ) ) ;
#18037 = CARTESIAN_POINT ( 'NONE',  ( -20.86347087121333388, -1.205278475425912932, 9.206679495332496188 ) ) ;
#18038 = VERTEX_POINT ( 'NONE', #22561 ) ;
#18039 = DIRECTION ( 'NONE',  ( 1.000000000000000000, 0.000000000000000000, 0.000000000000000000 ) ) ;
#18040 = CARTESIAN_POINT ( 'NONE',  ( 0.000000000000000000, 15.00000000000000000, 0.000000000000000000 ) ) ;
#18041 = CIRCLE ( 'NONE', #2949, 4.000000000000000000 ) ;
#18042 = CARTESIAN_POINT ( 'NONE',  ( 13.28343892131000104, -9.177482186369001482, 2.922696180057999804 ) ) ;
#18043 = CARTESIAN_POINT ( 'NONE',  ( 18.44601586413295990, 9.834069045321928826, -3.450538262810350698 ) ) ;
#18044 = EDGE_LOOP ( 'NONE', ( #1372, #23848, #6652, #8529 ) ) ;
#18045 = CARTESIAN_POINT ( 'NONE',  ( 1.536366799937286087, 28.51666666666666927, -1.999167105995451665 ) ) ;
#18046 = CARTESIAN_POINT ( 'NONE',  ( 2.575680369362000288, 29.21781557969000076, 0.8860769631535000412 ) ) ;
#18047 = DIRECTION ( 'NONE',  ( 1.000000000000000000, 0.000000000000000000, 0.000000000000000000 ) ) ;
#18048 = CARTESIAN_POINT ( 'NONE',  ( 4.750000000000000000, 17.00000000000000000, 0.000000000000000000 ) ) ;
#18049 = ORIENTED_EDGE ( 'NONE', *, *, #21996, .T. ) ;
#18050 = CONICAL_SURFACE ( 'NONE', #13770, 3.049999825846000157, 0.7853981633972997312 ) ;
#18051 = CARTESIAN_POINT ( 'NONE',  ( -10.35615758860000035, -1.075999958835999899E-14, 7.000000000000000000 ) ) ;
#18052 = DIRECTION ( 'NONE',  ( 0.000000000000000000, 0.4362437346113740011, -0.8998285414523820025 ) ) ;
#18053 = CARTESIAN_POINT ( 'NONE',  ( 15.91833333333333300, 4.572865580834726273, 7.933737425283369227 ) ) ;
#18054 = CARTESIAN_POINT ( 'NONE',  ( -23.90159383812773086, -3.635517970721634295, 9.022299759201507285 ) ) ;
#18055 = DIRECTION ( 'NONE',  ( 1.000000000000000000, 0.000000000000000000, 0.000000000000000000 ) ) ;
#18056 = CARTESIAN_POINT ( 'NONE',  ( 0.000000000000000000, 15.00000000000000000, -4.649999999999999467 ) ) ;
#18057 = CARTESIAN_POINT ( 'NONE',  ( -3.735429536209002865, 12.03300774351999713, 3.212544806379001638 ) ) ;
#18058 = CARTESIAN_POINT ( 'NONE',  ( 19.83062270046332642, 4.623427443748358456, 8.021463006140603369 ) ) ;
#18059 = ORIENTED_EDGE ( 'NONE', *, *, #10475, .T. ) ;
#18060 = DIRECTION ( 'NONE',  ( 0.000000000000000000, 1.000000000000000000, 0.000000000000000000 ) ) ;
#18061 = AXIS2_PLACEMENT_3D ( 'NONE', #12347, #10407, #1437 ) ;
#18062 = DIRECTION ( 'NONE',  ( 0.000000000000000000, 0.000000000000000000, -1.000000000000000000 ) ) ;
#18063 = AXIS2_PLACEMENT_3D ( 'NONE', #7813, #16765, #18952 ) ;
#18064 = VERTEX_POINT ( 'NONE', #2679 ) ;
#18065 = CARTESIAN_POINT ( 'NONE',  ( 6.132134859666997784, 14.49476015624998482, -0.03567915623813002618 ) ) ;
#18066 = CARTESIAN_POINT ( 'NONE',  ( 12.40357033523132912, 5.939957768465679244, -12.49999999999918288 ) ) ;
#18067 = CARTESIAN_POINT ( 'NONE',  ( 6.189458490575474592, 13.92434823838417479, -0.7784157444028274586 ) ) ;
#18068 = DIRECTION ( 'NONE',  ( 0.000000000000000000, 1.000000000000000000, 0.000000000000000000 ) ) ;
#18069 = DIRECTION ( 'NONE',  ( 0.000000000000000000, 1.000000000000000000, 0.000000000000000000 ) ) ;
#18070 = AXIS2_PLACEMENT_3D ( 'NONE', #6968, #20051, #3467 ) ;
#18071 = ORIENTED_EDGE ( 'NONE', *, *, #11135, .T. ) ;
#18072 = PLANE ( 'NONE',  #10051 ) ;
#18073 = CARTESIAN_POINT ( 'NONE',  ( -1.875162437998086684, 26.21985616695894450, 0.9907346142373321118 ) ) ;
#18074 = CONICAL_SURFACE ( 'NONE', #21934, 4.699999872533999756, 0.7853981633972997312 ) ;
#18075 = DIRECTION ( 'NONE',  ( 0.000000000000000000, 0.7956974229606958993, -0.6056943214969968681 ) ) ;
#18076 = ORIENTED_EDGE ( 'NONE', *, *, #8818, .F. ) ;
#18077 = CARTESIAN_POINT ( 'NONE',  ( -24.20325734908000115, -5.220886106840999297, -9.439784460628999341 ) ) ;
#18078 = AXIS2_PLACEMENT_3D ( 'NONE', #9091, #14653, #16700 ) ;
#18079 = CARTESIAN_POINT ( 'NONE',  ( -0.3502059142650872370, 28.20197603011382981, -4.416610674644638301 ) ) ;
#18080 = CARTESIAN_POINT ( 'NONE',  ( 14.54094227179021992, 2.725430164165235425, -9.955622680467328678 ) ) ;
#18081 = CARTESIAN_POINT ( 'NONE',  ( -12.25000000000000000, 1.374666032043000015E-14, 0.000000000000000000 ) ) ;
#18082 = CARTESIAN_POINT ( 'NONE',  ( 23.20815793052999965, -0.2658484307651000078, -11.27637876372000036 ) ) ;
#18083 = ADVANCED_FACE ( 'NONE', ( #969 ), #18556, .F. ) ;
#18084 = CARTESIAN_POINT ( 'NONE',  ( -1.901491585825000108, 30.15429474195000026, 1.041399949541000014 ) ) ;
#18085 = CARTESIAN_POINT ( 'NONE',  ( -10.34021276376999943, 1.351277883783999990E-14, 0.000000000000000000 ) ) ;
#18086 = CARTESIAN_POINT ( 'NONE',  ( -0.5822634062851997916, 11.56436112468998623, -4.714933848958999363 ) ) ;
#18087 = EDGE_LOOP ( 'NONE', ( #7956, #17353, #7685 ) ) ;
#18088 = DIRECTION ( 'NONE',  ( 0.000000000000000000, 1.000000000000000000, 0.000000000000000000 ) ) ;
#18089 = ORIENTED_EDGE ( 'NONE', *, *, #7730, .F. ) ;
#18090 = CARTESIAN_POINT ( 'NONE',  ( -2.184465970885646424, 29.53333333333333144, -1.259047450927245126 ) ) ;
#18091 = DIRECTION ( 'NONE',  ( 0.000000000000000000, 1.000000000000000000, 0.000000000000000000 ) ) ;
#18092 = CONICAL_SURFACE ( 'NONE', #5323, 4.309401076758999416, 1.119376321708719590 ) ;
#18093 = ORIENTED_EDGE ( 'NONE', *, *, #12820, .F. ) ;
#18094 = CARTESIAN_POINT ( 'NONE',  ( -12.25000000000000000, 1.374666032043000015E-14, 0.000000000000000000 ) ) ;
#18095 = CARTESIAN_POINT ( 'NONE',  ( 17.35441666666665839, 8.879300184524714368, -2.386375964361124424 ) ) ;
#18096 = ADVANCED_FACE ( 'NONE', ( #10068 ), #15046, .F. ) ;
#18097 = AXIS2_PLACEMENT_3D ( 'NONE', #19853, #3026, #10888 ) ;
#18098 = CARTESIAN_POINT ( 'NONE',  ( 21.38008103379665314, 9.219936730289768789, 1.206759948112953618 ) ) ;
#18099 = CARTESIAN_POINT ( 'NONE',  ( 24.45564077607145492, 2.060124049349388642, -12.50000000000000355 ) ) ;
#18100 = AXIS2_PLACEMENT_3D ( 'NONE', #22954, #13394, #6371 ) ;
#18101 = CARTESIAN_POINT ( 'NONE',  ( 2.052373795670999979, 28.06006359723999921, -1.371352433351999744 ) ) ;
#18102 = VERTEX_POINT ( 'NONE', #14057 ) ;
#18103 = CARTESIAN_POINT ( 'NONE',  ( -9.894391138769998761, -12.85207681411000102, 8.150135934440999819 ) ) ;
#18104 = CARTESIAN_POINT ( 'NONE',  ( 13.50000000000000178, 7.201649267261895915, -5.777227494228245774 ) ) ;
#18105 = CARTESIAN_POINT ( 'NONE',  ( -14.25243324638999809, -13.93375672974000068, -0.8660254037843999608 ) ) ;
#18106 = ORIENTED_EDGE ( 'NONE', *, *, #14312, .T. ) ;
#18107 = DIRECTION ( 'NONE',  ( 0.000000000000000000, 1.000000000000000000, 0.000000000000000000 ) ) ;
#18108 = CARTESIAN_POINT ( 'NONE',  ( 22.58815793041088682, -5.572103469424654065, 8.998486307808107654 ) ) ;
#18109 = CARTESIAN_POINT ( 'NONE',  ( -14.00000000000000178, 7.473072963007769687, 5.353906094287523842 ) ) ;
#18110 = CARTESIAN_POINT ( 'NONE',  ( 17.54864771944206936, -9.976641182250055806, 3.124397047610406819 ) ) ;
#18111 = AXIS2_PLACEMENT_3D ( 'NONE', #10506, #5171, #14480 ) ;
#18112 = CIRCLE ( 'NONE', #20042, 12.49999999999999289 ) ;
#18113 = CARTESIAN_POINT ( 'NONE',  ( -18.75303743917333321, -1.198189225339903352, 9.152521614020351137 ) ) ;
#18114 = EDGE_CURVE ( 'NONE', #2392, #17545, #7576, .T. ) ;
#18115 = CARTESIAN_POINT ( 'NONE',  ( 1.316912383867000047, 30.51493852343000412, 1.747677774086999980 ) ) ;
#18116 = CARTESIAN_POINT ( 'NONE',  ( -13.32041877100999905, -7.827390682981001824, 5.681961735881999154 ) ) ;
#18117 = CARTESIAN_POINT ( 'NONE',  ( 1.721625935243284999, 29.88644617415637228, -1.304246024930588721 ) ) ;
#18118 = ORIENTED_EDGE ( 'NONE', *, *, #15284, .F. ) ;
#18119 = CARTESIAN_POINT ( 'NONE',  ( -24.24003052284658466, -3.589673254547931514, 12.49985157730626284 ) ) ;
#18120 = CARTESIAN_POINT ( 'NONE',  ( 23.42416300332000034, 1.450584581381999971, -11.39090740897000131 ) ) ;
#18121 = CARTESIAN_POINT ( 'NONE',  ( 22.42725290643797109, 6.724562262194361040, 8.161878525604194579 ) ) ;
#18122 = CARTESIAN_POINT ( 'NONE',  ( -8.099999999999999645, -10.50000000000000000, -1.882608235970000037E-09 ) ) ;
#18123 = ORIENTED_EDGE ( 'NONE', *, *, #5383, .F. ) ;
#18124 = FACE_OUTER_BOUND ( 'NONE', #23475, .T. ) ;
#18125 = DIRECTION ( 'NONE',  ( -1.000000000000000000, 0.000000000000000000, 0.000000000000000000 ) ) ;
#18126 = EDGE_CURVE ( 'NONE', #7614, #1045, #21329, .T. ) ;
#18127 = CONICAL_SURFACE ( 'NONE', #17742, 9.161549281532000322, 0.02565634000431304615 ) ;
#18128 = CARTESIAN_POINT ( 'NONE',  ( -4.558962899038999872, 12.31676645013000915, -1.631911765495000166 ) ) ;
#18129 = ORIENTED_EDGE ( 'NONE', *, *, #1582, .F. ) ;
#18130 = CARTESIAN_POINT ( 'NONE',  ( 15.99918875730999979, 7.956028365285000348, 4.607548929765999723 ) ) ;
#18131 = ORIENTED_EDGE ( 'NONE', *, *, #3187, .T. ) ;
#18132 = CARTESIAN_POINT ( 'NONE',  ( 2.177371421982348121, 27.24903633706587769, -0.3268671095024456852 ) ) ;
#18133 = CONTEXT_DEPENDENT_SHAPE_REPRESENTATION ( #16830, #9387 ) ;
#18134 = EDGE_CURVE ( 'NONE', #4988, #551, #3928, .T. ) ;
#18135 = CARTESIAN_POINT ( 'NONE',  ( -23.74465998031000069, -13.93375672974000068, -0.8660254037843999608 ) ) ;
#18136 = AXIS2_PLACEMENT_3D ( 'NONE', #12936, #20334, #7249 ) ;
#18137 = ORIENTED_EDGE ( 'NONE', *, *, #19301, .T. ) ;
#18138 = CARTESIAN_POINT ( 'NONE',  ( -19.06933321534334169, -0.5773117834577096152, 9.204639638764268383 ) ) ;
#18139 = AXIS2_PLACEMENT_3D ( 'NONE', #19315, #22928, #2725 ) ;
#18140 = CARTESIAN_POINT ( 'NONE',  ( -21.54615255932999673, -7.601428298414999674, -6.679749176401998945 ) ) ;
#18141 = EDGE_CURVE ( 'NONE', #11746, #18064, #2119, .T. ) ;
#18142 = CARTESIAN_POINT ( 'NONE',  ( 0.000000000000000000, 28.00000000000000000, 0.000000000000000000 ) ) ;
#18143 = FACE_OUTER_BOUND ( 'NONE', #17490, .T. ) ;
#18144 = EDGE_CURVE ( 'NONE', #4139, #21511, #13407, .T. ) ;
#18145 = CARTESIAN_POINT ( 'NONE',  ( -22.38871519940780175, 8.023834466003746613, -7.050152665355915005 ) ) ;
#18146 = CARTESIAN_POINT ( 'NONE',  ( 1.684526538292457465, 28.11547461990329211, 1.425451057090266982 ) ) ;
#18147 = VECTOR ( 'NONE', #18438, 1000.000000000000000 ) ;
#18148 = CARTESIAN_POINT ( 'NONE',  ( -6.248053578788996809, 15.23699721607000868, 1.996732876636001963 ) ) ;
#18149 = CARTESIAN_POINT ( 'NONE',  ( -0.7318187998270078154, 29.87490599056237528, 4.196286372439439027 ) ) ;
#18150 = EDGE_LOOP ( 'NONE', ( #18330, #194, #14116, #7492, #18243 ) ) ;
#18151 = CARTESIAN_POINT ( 'NONE',  ( -17.46222087121334710, 5.604205574924105093, 7.292568942664221510 ) ) ;
#18152 = CARTESIAN_POINT ( 'NONE',  ( 2.040326213578687486, 26.33271864848902055, 0.9387218070561216265 ) ) ;
#18153 = CARTESIAN_POINT ( 'NONE',  ( 0.3985328791175999918, 26.36619850838000190, 2.231710853292999897 ) ) ;
#18154 = AXIS2_PLACEMENT_3D ( 'NONE', #2544, #17450, #17696 ) ;
#18155 = CARTESIAN_POINT ( 'NONE',  ( -24.47329604352722754, -7.448162605973902117, -7.555104833657267704 ) ) ;
#18156 = CARTESIAN_POINT ( 'NONE',  ( 0.9420013681046000009, 28.89271896306000187, 1.848781781241999989 ) ) ;
#18157 = EDGE_CURVE ( 'NONE', #15650, #6003, #19874, .T. ) ;
#18158 = AXIS2_PLACEMENT_3D ( 'NONE', #22695, #7697, #16888 ) ;
#18159 = CARTESIAN_POINT ( 'NONE',  ( 3.761864348328608720, 12.07395163634499546, 3.036815456826709614 ) ) ;
#18160 = VERTEX_POINT ( 'NONE', #21450 ) ;
#18161 = CARTESIAN_POINT ( 'NONE',  ( 17.80791666666665662, 2.389422108709928327, 8.890634990046439867 ) ) ;
#18162 = CARTESIAN_POINT ( 'NONE',  ( 2.541275575112173613, 11.75631033188225771, -4.097795235817846660 ) ) ;
#18163 = CARTESIAN_POINT ( 'NONE',  ( -10.04701370329000021, 16.31160201364000173, 0.9999999999983000265 ) ) ;
#18164 = CIRCLE ( 'NONE', #22388, 10.59999999999999964 ) ;
#18165 = CARTESIAN_POINT ( 'NONE',  ( -20.52334587121333698, -8.958601747919349378, 2.407426987275048891 ) ) ;
#18166 = ORIENTED_EDGE ( 'NONE', *, *, #19913, .F. ) ;
#18167 = FACE_OUTER_BOUND ( 'NONE', #2304, .T. ) ;
#18168 = CARTESIAN_POINT ( 'NONE',  ( -9.000000000000000000, 19.50000000000000000, -6.000000000000000000 ) ) ;
#18169 = CARTESIAN_POINT ( 'NONE',  ( 15.03843892131000004, -8.433581200277000534, 4.746982932527000543 ) ) ;
#18170 = CARTESIAN_POINT ( 'NONE',  ( 18.70320243966950358, 8.881428319331240218, 5.464808494914835002 ) ) ;
#18171 = UNCERTAINTY_MEASURE_WITH_UNIT (LENGTH_MEASURE( 1.000000000000000082E-05 ), #5688, 'distance_accuracy_value', 'NONE');
#18172 = DIRECTION ( 'NONE',  ( 1.000000000000000000, 0.000000000000000000, 0.000000000000000000 ) ) ;
#18173 = CARTESIAN_POINT ( 'NONE',  ( 0.2320996736816000328, 30.35746553841000051, 2.138195049080999777 ) ) ;
#18174 = CARTESIAN_POINT ( 'NONE',  ( 18.91608580085999947, 1.014672566925000075, 11.40123757166999852 ) ) ;
#18175 = CARTESIAN_POINT ( 'NONE',  ( -23.74465998031000069, -13.93375672974000068, 0.8660254037843999608 ) ) ;
#18176 = AXIS2_PLACEMENT_3D ( 'NONE', #15966, #17690, #17931 ) ;
#18177 = VERTEX_POINT ( 'NONE', #5108 ) ;
#18178 = VECTOR ( 'NONE', #22253, 1000.000000000000114 ) ;
#18179 = DIRECTION ( 'NONE',  ( 0.000000000000000000, 1.000000000000000000, 0.000000000000000000 ) ) ;
#18180 = CARTESIAN_POINT ( 'NONE',  ( 20.04180759019999769, -2.870714866723000025, -10.33318544762000002 ) ) ;
#18181 = LINE ( 'NONE', #7247, #18178 ) ;
#18182 = PLANE ( 'NONE',  #12340 ) ;
#18183 = CARTESIAN_POINT ( 'NONE',  ( -11.00000000000000000, 1.359357947053999856E-14, 0.000000000000000000 ) ) ;
#18184 = DIRECTION ( 'NONE',  ( 0.000000000000000000, -1.000000000000000000, 0.000000000000000000 ) ) ;
#18185 = DIRECTION ( 'NONE',  ( 0.000000000000000000, 1.000000000000000000, 0.000000000000000000 ) ) ;
#18186 = VERTEX_POINT ( 'NONE', #10795 ) ;
#18187 = EDGE_CURVE ( 'NONE', #9372, #9495, #4835, .T. ) ;
#18188 = DIRECTION ( 'NONE',  ( 1.000000000000000000, 0.000000000000000000, 0.000000000000000000 ) ) ;
#18189 = CARTESIAN_POINT ( 'NONE',  ( -4.000000000000000000, 26.31534065533125144, 1.802053058880663805 ) ) ;
#18190 = ORIENTED_EDGE ( 'NONE', *, *, #2527, .T. ) ;
#18191 = AXIS2_PLACEMENT_3D ( 'NONE', #9469, #11650, #5830 ) ;
#18192 = CARTESIAN_POINT ( 'NONE',  ( -1.907767351274999967, 24.04667396097999799, 1.684751507996000042 ) ) ;
#18193 = DIRECTION ( 'NONE',  ( 0.000000000000000000, -1.000000000000000000, 0.000000000000000000 ) ) ;
#18194 = CARTESIAN_POINT ( 'NONE',  ( 11.53663804754732602, 3.465671449080339972, -12.49990775415077238 ) ) ;
#18195 = CARTESIAN_POINT ( 'NONE',  ( 6.225415451459330285, 13.76263273567627721, -1.301510523365907668 ) ) ;
#18196 = DIRECTION ( 'NONE',  ( 0.000000000000000000, 0.000000000000000000, -1.000000000000000000 ) ) ;
#18197 = CARTESIAN_POINT ( 'NONE',  ( -6.045497365604999729, 16.31815993523999708, -1.000000000000000000 ) ) ;
#18198 = EDGE_LOOP ( 'NONE', ( #12607, #7551, #2439 ) ) ;
#18199 = DIRECTION ( 'NONE',  ( 0.000000000000000000, 1.000000000000000000, 0.000000000000000000 ) ) ;
#18200 = AXIS2_PLACEMENT_3D ( 'NONE', #13402, #20803, #21037 ) ;
#18201 = CARTESIAN_POINT ( 'NONE',  ( -1.963703823225463774, 26.25920717875808563, 0.8995588027868727243 ) ) ;
#18202 = CYLINDRICAL_SURFACE ( 'NONE', #20573, 6.125000000000000000 ) ;
#18203 = ORIENTED_EDGE ( 'NONE', *, *, #5972, .F. ) ;
#18204 = CARTESIAN_POINT ( 'NONE',  ( -10.32558623928693464, 15.68963668235006459, -1.216814257780576503 ) ) ;
#18205 = CARTESIAN_POINT ( 'NONE',  ( 1.244068065386999988, 24.76929142835999897, 1.746894613178000100 ) ) ;
#18206 = CARTESIAN_POINT ( 'NONE',  ( 14.76281341799735536, 8.902647515865099948, -5.236912464659464916 ) ) ;
#18207 = LINE ( 'NONE', #10332, #11414 ) ;
#18208 = CARTESIAN_POINT ( 'NONE',  ( 23.02461096755999748, -6.906568182436000569, -8.911400877533001363 ) ) ;
#18209 = DIRECTION ( 'NONE',  ( 0.000000000000000000, 0.000000000000000000, -1.000000000000000000 ) ) ;
#18210 = CARTESIAN_POINT ( 'NONE',  ( 14.38895978305333223, -4.028520541369379870, 8.094092768459281828 ) ) ;
#18211 = DIRECTION ( 'NONE',  ( 0.000000000000000000, 0.000000000000000000, -1.000000000000000000 ) ) ;
#18212 = CARTESIAN_POINT ( 'NONE',  ( -21.77047087121331614, 1.208325219156647146, -9.229954902935974204 ) ) ;
#18213 = ORIENTED_EDGE ( 'NONE', *, *, #23467, .T. ) ;
#18214 = DIRECTION ( 'NONE',  ( 0.000000000000000000, -1.000000000000000000, 0.000000000000000000 ) ) ;
#18215 = EDGE_LOOP ( 'NONE', ( #12988, #13754, #16696, #7611 ) ) ;
#18216 = CARTESIAN_POINT ( 'NONE',  ( 11.78924557931885886, -12.98180138940026396, -2.514846131778560867 ) ) ;
#18217 = DIRECTION ( 'NONE',  ( 0.000000000000000000, 0.000000000000000000, 1.000000000000000000 ) ) ;
#18218 = CARTESIAN_POINT ( 'NONE',  ( 16.85852266364000229, 0.2855060302065000055, 11.07656398360000161 ) ) ;
#18219 = EDGE_CURVE ( 'NONE', #21511, #10829, #7524, .T. ) ;
#18220 = ORIENTED_EDGE ( 'NONE', *, *, #2718, .F. ) ;
#18221 = CARTESIAN_POINT ( 'NONE',  ( -8.985362565845999683, 11.16660274832999988, -9.816446337639002095 ) ) ;
#18222 = CARTESIAN_POINT ( 'NONE',  ( 13.49999999999999467, 7.950735579686481813, -4.793967810291187348 ) ) ;
#18223 = CARTESIAN_POINT ( 'NONE',  ( -14.25546672378000146, -6.466739220293000301, 12.35574276786000070 ) ) ;
#18224 = ORIENTED_EDGE ( 'NONE', *, *, #8958, .T. ) ;
#18225 = CARTESIAN_POINT ( 'NONE',  ( 20.55855148008149413, 2.013822818936180425, 10.33642651244847599 ) ) ;
#18226 = CARTESIAN_POINT ( 'NONE',  ( 12.50448119322000018, -13.93375672974000068, 0.4328388268750000267 ) ) ;
#18227 = CARTESIAN_POINT ( 'NONE',  ( 15.97809595731088450, -8.909303387638358274, -5.284970025649013969 ) ) ;
#18228 = CARTESIAN_POINT ( 'NONE',  ( -5.345626673175369881, 14.28230134421816722, 5.048067894539765454 ) ) ;
#18229 = CARTESIAN_POINT ( 'NONE',  ( -1.706122057262999814, 30.94656064747999835, -1.370363639857999916 ) ) ;
#18230 = FACE_OUTER_BOUND ( 'NONE', #9853, .T. ) ;
#18231 = CARTESIAN_POINT ( 'NONE',  ( 2.127842856066609389, 29.82575304422995899, -0.3714889427421172452 ) ) ;
#18232 = ORIENTED_EDGE ( 'NONE', *, *, #12310, .T. ) ;
#18233 = CARTESIAN_POINT ( 'NONE',  ( 20.46948943370828999, 9.758937805927079268, 3.938997005426223996 ) ) ;
#18234 = DIRECTION ( 'NONE',  ( -1.734723475976817507E-14, -1.000000000000000000, -1.792960224734025295E-10 ) ) ;
#18235 = ORIENTED_EDGE ( 'NONE', *, *, #9109, .F. ) ;
#18236 = CARTESIAN_POINT ( 'NONE',  ( -2.102266727616999731, 23.66000000000000014, 0.4960590750638999569 ) ) ;
#18237 = CARTESIAN_POINT ( 'NONE',  ( -1.989999999999999991, 9.799994897958001161, -7.500000000000000000 ) ) ;
#18238 = B_SPLINE_CURVE_WITH_KNOTS ( 'NONE', 3,
 ( #14556, #5362, #21949, #12751, #3550, #10934, #20143, #12972, #23875, #18320, #7281, #1726, #22069, #5592, #14675, #5477, #20257, #19365, #15831, #10274, #23219, #21417, #19485, #15132, #2187, #12217, #9580, #17542, #22974, #15946, #23092, #14026, #21542, #19607, #17795, #1191, #18778 ),
 .UNSPECIFIED., .F., .F.,
 ( 4, 2, 2, 2, 2, 2, 2, 2, 2, 2, 1, 1, 2, 2, 1, 2, 2, 2, 2, 4 ),
 ( 0.000000000000000000, 0.1115186113371554461, 0.1672779170057331344, 0.2230372226743108366, 0.2787965283428885943, 0.3345558340114662688, 0.3903151396800439987, 0.4460744453486216732, 0.4739540981829105659, 0.4878939246000549290, 0.4948638378086272493, 0.4983487944129132985, 0.4992200335639848108, 0.5000912727150563786, 0.5018337510171992921, 0.5575930566857747461, 0.6133523623543503112, 0.6691116680229257652, 0.7806302793600768952, 0.8921488906972279143 ),
 .UNSPECIFIED. ) ;
#18239 = CARTESIAN_POINT ( 'NONE',  ( -1.429747209652000084, 11.58582448925999131, -4.584039058762003016 ) ) ;
#18240 = VERTEX_POINT ( 'NONE', #3290 ) ;
#18241 = ADVANCED_FACE ( 'NONE', ( #8612 ), #17589, .T. ) ;
#18242 = CARTESIAN_POINT ( 'NONE',  ( 0.000000000000000000, 17.00000000000000000, 0.000000000000000000 ) ) ;
#18243 = ORIENTED_EDGE ( 'NONE', *, *, #18731, .F. ) ;
#18244 = B_SPLINE_CURVE_WITH_KNOTS ( 'NONE', 3,
 ( #6634, #937, #19733, #4830, #12099, #17663, #6515, #12216, #8461, #21416, #16067, #19364, #19606, #6754, #23091, #17541, #8583, #14025 ),
 .UNSPECIFIED., .F., .F.,
 ( 4, 2, 2, 2, 2, 2, 2, 2, 4 ),
 ( 0.000000000000000000, 0.1249999999999998612, 0.2499999999999997224, 0.3749999999999996114, 0.4999999999999996669, 0.6249999999999997780, 0.7499999999999997780, 0.8749999999999998890, 1.000000000000000000 ),
 .UNSPECIFIED. ) ;
#18245 = CARTESIAN_POINT ( 'NONE',  ( -5.182227472513371680, 15.97908023997939075, 3.265408057167412448 ) ) ;
#18246 = CARTESIAN_POINT ( 'NONE',  ( -14.45529023501843824, 2.584742736972815536, -12.49997119545760782 ) ) ;
#18247 = ORIENTED_EDGE ( 'NONE', *, *, #15909, .F. ) ;
#18248 = CARTESIAN_POINT ( 'NONE',  ( -15.38367920454667370, -2.373138586668962713, 8.830043457142039642 ) ) ;
#18249 = CARTESIAN_POINT ( 'NONE',  ( -21.06439250443000333, 7.381144841870000306, -6.903346092959000480 ) ) ;
#18250 = EDGE_CURVE ( 'NONE', #10960, #1186, #19911, .T. ) ;
#18251 = CARTESIAN_POINT ( 'NONE',  ( 12.40357033524515451, -7.855338663056838477, -11.39415432492425850 ) ) ;
#18252 = CARTESIAN_POINT ( 'NONE',  ( -6.370829674278999377, 15.09915248894001749, -3.226228642116999001 ) ) ;
#18253 = CARTESIAN_POINT ( 'NONE',  ( -22.69753670837523885, -2.324815390030910756, -10.30365430221285905 ) ) ;
#18254 = CARTESIAN_POINT ( 'NONE',  ( 1.948395284584199638, 28.14197577173313292, 1.033326755142028430 ) ) ;
#18255 = CARTESIAN_POINT ( 'NONE',  ( -1.500144717171000064, 28.73000240009999828, -2.447990496630999768 ) ) ;
#18256 = CARTESIAN_POINT ( 'NONE',  ( -1.678813317411953054, 30.00000000000000355, 3.649538832790644616 ) ) ;
#18257 = ORIENTED_EDGE ( 'NONE', *, *, #3368, .T. ) ;
#18258 = DIRECTION ( 'NONE',  ( 0.000000000000000000, 1.000000000000000000, 0.000000000000000000 ) ) ;
#18259 = DIRECTION ( 'NONE',  ( 0.000000000000000000, -1.000000000000000000, 0.000000000000000000 ) ) ;
#18260 = CARTESIAN_POINT ( 'NONE',  ( 14.96234510379274418, -9.055474543150360489, 0.9759141728302277441 ) ) ;
#18261 = B_SPLINE_CURVE_WITH_KNOTS ( 'NONE', 3,
 ( #1928, #5303, #18371, #17911, #21666, #8943, #18264, #9170, #3380, #16425, #12694, #23814, #1782, #6997, #8831, #14386 ),
 .UNSPECIFIED., .F., .F.,
 ( 4, 2, 2, 1, 1, 1, 1, 2, 2, 4 ),
 ( 0.000000000000000000, 0.2500000000000089373, 0.3750000000000134892, 0.4375000000000157097, 0.4687500000000168199, 0.4843750000000172640, 0.4921875000000175415, 0.4960937500000173750, 0.5000000000000172085, 1.000000000000000000 ),
 .UNSPECIFIED. ) ;
#18262 = EDGE_CURVE ( 'NONE', #479, #14961, #23623, .T. ) ;
#18263 = AXIS2_PLACEMENT_3D ( 'NONE', #12014, #17206, #21084 ) ;
#18264 = CARTESIAN_POINT ( 'NONE',  ( 5.895600255881173091, 14.43378529329739202, -1.663721376250851591 ) ) ;
#18265 = CARTESIAN_POINT ( 'NONE',  ( -0.6636689712800000196, 28.79521896306000173, 2.189073617939000016 ) ) ;
#18266 = LINE ( 'NONE', #7349, #21659 ) ;
#18267 = ORIENTED_EDGE ( 'NONE', *, *, #10127, .T. ) ;
#18268 = ADVANCED_FACE ( 'NONE', ( #14179 ), #18732, .T. ) ;
#18269 = CARTESIAN_POINT ( 'NONE',  ( -3.028157117397000331, 11.86875440406517157, -3.760788192032637589 ) ) ;
#18270 = CARTESIAN_POINT ( 'NONE',  ( 24.22902234330208771, 5.299939913159104954, -8.069587291013673891 ) ) ;
#18271 = AXIS2_PLACEMENT_3D ( 'NONE', #4354, #16947, #115 ) ;
#18272 = CARTESIAN_POINT ( 'NONE',  ( 2.202166145775246164, 29.66321151848345394, -0.5828424432849000913 ) ) ;
#18273 = ORIENTED_EDGE ( 'NONE', *, *, #3908, .T. ) ;
#18274 = CARTESIAN_POINT ( 'NONE',  ( 2.500000000000001332, 24.38333333333333641, 0.3272492347489234787 ) ) ;
#18275 = CARTESIAN_POINT ( 'NONE',  ( -14.25394822846000054, 13.93375672974000068, -0.7219352443379000173 ) ) ;
#18276 = CARTESIAN_POINT ( 'NONE',  ( 17.36831408530999710, -9.345903658884999743, -4.204539402675000481 ) ) ;
#18277 = CARTESIAN_POINT ( 'NONE',  ( 18.58914845423001694, 10.30955476201900112, 1.554838316117926222 ) ) ;
#18278 = ADVANCED_FACE ( 'NONE', ( #23733 ), #17190, .F. ) ;
#18279 = LINE ( 'NONE', #18386, #729 ) ;
#18280 = CARTESIAN_POINT ( 'NONE',  ( 1.754903278477999873, 30.62218442030999910, -1.243399122562000025 ) ) ;
#18281 = CARTESIAN_POINT ( 'NONE',  ( -12.51334610648000023, 6.705591387245999790, -5.997258770121999483 ) ) ;
#18282 = CARTESIAN_POINT ( 'NONE',  ( 13.50000000000000178, -7.857961930001017059, 6.282614375059098144 ) ) ;
#18283 = AXIS2_PLACEMENT_3D ( 'NONE', #2087, #22432, #11062 ) ;
#18284 = EDGE_LOOP ( 'NONE', ( #1723, #19589, #2955, #9501 ) ) ;
#18285 = FACE_OUTER_BOUND ( 'NONE', #13377, .T. ) ;
#18286 = CARTESIAN_POINT ( 'NONE',  ( 19.51066028373000094, -9.186672159909999635, 5.505812582796999699 ) ) ;
#18287 = DIRECTION ( 'NONE',  ( 0.000000000000000000, 1.000000000000000000, 0.000000000000000000 ) ) ;
#18288 = CARTESIAN_POINT ( 'NONE',  ( 13.77884874240669433, -10.28178801782097374, 1.171900820996238490 ) ) ;
#18289 = DIRECTION ( 'NONE',  ( 0.9063077870366585964, 0.000000000000000000, 0.4226182617406808451 ) ) ;
#18290 = CARTESIAN_POINT ( 'NONE',  ( -4.720810408942003988, 12.43069267676998635, 1.485243188514001833 ) ) ;
#18291 = CARTESIAN_POINT ( 'NONE',  ( 0.2552732384256292120, 29.18862125910514038, -2.144907518227253007 ) ) ;
#18292 = CARTESIAN_POINT ( 'NONE',  ( -12.25000000000000000, 9.358908280841877314, -11.49204783487746617 ) ) ;
#18293 = EDGE_LOOP ( 'NONE', ( #21219, #2243, #18839, #14752 ) ) ;
#18294 = CARTESIAN_POINT ( 'NONE',  ( 0.000000000000000000, 22.09999988306816832, 0.000000000000000000 ) ) ;
#18295 = ORIENTED_EDGE ( 'NONE', *, *, #10087, .F. ) ;
#18296 = CARTESIAN_POINT ( 'NONE',  ( -1.619994985406000065, 23.83580469984000061, 1.430619405864999916 ) ) ;
#18297 = ADVANCED_FACE ( 'NONE', ( #14415 ), #3173, .T. ) ;
#18298 = CARTESIAN_POINT ( 'NONE',  ( 2.184465970885649977, 28.33333333333333570, 1.259047450927240686 ) ) ;
#18299 = CARTESIAN_POINT ( 'NONE',  ( 4.151454423752853451, 13.37950420772049043, 5.414973749174229134 ) ) ;
#18300 = EDGE_CURVE ( 'NONE', #3092, #11881, #9900, .T. ) ;
#18301 = CONICAL_SURFACE ( 'NONE', #2036, 14.15464499511999996, 0.6126053401530057174 ) ;
#18302 = CARTESIAN_POINT ( 'NONE',  ( -5.916823184047997231, 16.44723308294000930, -1.645665246264000237 ) ) ;
#18303 = ORIENTED_EDGE ( 'NONE', *, *, #20745, .F. ) ;
#18304 = FACE_OUTER_BOUND ( 'NONE', #10672, .T. ) ;
#18305 = CARTESIAN_POINT ( 'NONE',  ( -0.8800650012412046808, 26.22123020134747762, 1.934182370176196208 ) ) ;
#18306 = FACE_OUTER_BOUND ( 'NONE', #6, .T. ) ;
#18307 = EDGE_LOOP ( 'NONE', ( #697, #4334, #218, #23684 ) ) ;
#18308 = ADVANCED_FACE ( 'NONE', ( #1049 ), #9981, .F. ) ;
#18309 = CARTESIAN_POINT ( 'NONE',  ( -10.78142806654279084, 15.38209275545921173, -1.630562623988462079 ) ) ;
#18310 = EDGE_CURVE ( 'NONE', #8938, #21190, #14245, .T. ) ;
#18311 = CARTESIAN_POINT ( 'NONE',  ( 0.01836207933452999735, 24.98406236978999928, -2.335018217200000024 ) ) ;
#18312 = CARTESIAN_POINT ( 'NONE',  ( 14.55590497721902388, 3.259501315177474989, -9.794662651058661851 ) ) ;
#18313 = CYLINDRICAL_SURFACE ( 'NONE', #7149, 10.65000000000000036 ) ;
#18314 = CARTESIAN_POINT ( 'NONE',  ( 22.03302542056999869, 10.37153216069000017, -4.351098818476000218 ) ) ;
#18315 = CARTESIAN_POINT ( 'NONE',  ( 1.263588213801000171, 30.36972139875000209, 1.761683537874000116 ) ) ;
#18316 = CARTESIAN_POINT ( 'NONE',  ( 13.64892411898719615, 7.821303059129255608, -4.509097355506050953 ) ) ;
#18317 = CARTESIAN_POINT ( 'NONE',  ( -6.250000000000000000, 15.73203524433000311, -1.185075242810999852 ) ) ;
#18318 = SURFACE_SIDE_STYLE ('',( #10932 ) ) ;
#18319 = EDGE_LOOP ( 'NONE', ( #6081, #22254, #17232, #22686, #1907 ) ) ;
#18320 = CARTESIAN_POINT ( 'NONE',  ( -14.75505759937285610, -5.861744336721237403, -6.919050695072026080 ) ) ;
#18321 = FACE_OUTER_BOUND ( 'NONE', #19602, .T. ) ;
#18322 = AXIS2_PLACEMENT_3D ( 'NONE', #3333, #14914, #14796 ) ;
#18323 = ORIENTED_EDGE ( 'NONE', *, *, #9715, .F. ) ;
#18324 = LINE ( 'NONE', #7286, #9915 ) ;
#18325 = CARTESIAN_POINT ( 'NONE',  ( 11.09594815121266898, -10.32758188524896958, -7.112100880958000637 ) ) ;
#18326 = CARTESIAN_POINT ( 'NONE',  ( 21.53124770046332515, 7.376069553053762107, 5.668376081327591187 ) ) ;
#18327 = B_SPLINE_CURVE_WITH_KNOTS ( 'NONE', 3,
 ( #20182, #14715, #9040, #20297, #1769, #3943 ),
 .UNSPECIFIED., .F., .F.,
 ( 4, 2, 4 ),
 ( 0.000000000000000000, 0.1249467100871154007, 0.2498934201742307459 ),
 .UNSPECIFIED. ) ;
#18328 = CARTESIAN_POINT ( 'NONE',  ( 13.06905380888999879, 5.678881668803000160, 8.574739485425999064 ) ) ;
#18329 = CARTESIAN_POINT ( 'NONE',  ( -16.14924287180106788, 2.273826895442076168, 10.14427581049354288 ) ) ;
#18330 = ORIENTED_EDGE ( 'NONE', *, *, #8184, .T. ) ;
#18331 = CARTESIAN_POINT ( 'NONE',  ( -11.01443863877000062, -7.881785293157000716, -13.01837374353999977 ) ) ;
#18332 = DIRECTION ( 'NONE',  ( 0.000000000000000000, 0.000000000000000000, 1.000000000000000000 ) ) ;
#18333 = CARTESIAN_POINT ( 'NONE',  ( -14.25547010304999951, -7.466739166992000243, 11.77839252945000048 ) ) ;
#18334 = ORIENTED_EDGE ( 'NONE', *, *, #4623, .F. ) ;
#18335 = CARTESIAN_POINT ( 'NONE',  ( 22.70581627535820246, -8.684860224558871522, 6.045228987698447298 ) ) ;
#18336 = DIRECTION ( 'NONE',  ( -1.000000000000000000, 0.000000000000000000, 0.000000000000000000 ) ) ;
#18337 = CARTESIAN_POINT ( 'NONE',  ( 15.97136033905609231, -9.035590316731877181, -5.065116864595969659 ) ) ;
#18338 = CARTESIAN_POINT ( 'NONE',  ( -17.36285270628999911, -10.99392015758999896, 1.404702108876000111 ) ) ;
#18339 = CARTESIAN_POINT ( 'NONE',  ( 0.5050338295773000308, 28.84204524523000046, 2.287831773294000115 ) ) ;
#18340 = CARTESIAN_POINT ( 'NONE',  ( -17.78928642635000301, 9.027876325972000515, -3.804579355723999967 ) ) ;
#18341 = CARTESIAN_POINT ( 'NONE',  ( -0.2273216873190004872, 30.01705067798956250, -2.154795586676287567 ) ) ;
#18342 = ORIENTED_EDGE ( 'NONE', *, *, #13389, .T. ) ;
#18343 = CARTESIAN_POINT ( 'NONE',  ( 2.234556666495999711, 24.25198102494999830, -0.6798364240153000893 ) ) ;
#18344 = CARTESIAN_POINT ( 'NONE',  ( 19.61828792382229381, -8.805202494819290848, -5.729946969217829533 ) ) ;
#18345 = CARTESIAN_POINT ( 'NONE',  ( -1.955724675740084795, 26.26076676662178855, 0.9180910909140133080 ) ) ;
#18346 = EDGE_LOOP ( 'NONE', ( #14507, #10019, #22168, #21936 ) ) ;
#18347 = CARTESIAN_POINT ( 'NONE',  ( -0.3136752098478812756, 23.81257023422828922, 2.231325233347782877 ) ) ;
#18348 = FACE_OUTER_BOUND ( 'NONE', #21488, .T. ) ;
#18349 = CARTESIAN_POINT ( 'NONE',  ( -4.778817678460002938, 12.40039738087000387, -0.7843833587508003413 ) ) ;
#18350 = ORIENTED_EDGE ( 'NONE', *, *, #13086, .F. ) ;
#18351 = CARTESIAN_POINT ( 'NONE',  ( 11.61168875731000050, -4.628380041800000733, -7.810153319783999848 ) ) ;
#18352 = CIRCLE ( 'NONE', #9069, 10.59999999999999964 ) ;
#18353 = ORIENTED_EDGE ( 'NONE', *, *, #22865, .T. ) ;
#18354 = CARTESIAN_POINT ( 'NONE',  ( -5.091933128512972750, 15.92787516682906634, 3.404252275490784463 ) ) ;
#18355 = DIRECTION ( 'NONE',  ( 0.000000000000000000, -1.000000000000000000, 9.414779719719000361E-11 ) ) ;
#18356 = ORIENTED_EDGE ( 'NONE', *, *, #9697, .F. ) ;
#18357 = CARTESIAN_POINT ( 'NONE',  ( 8.124934037954998800, 14.44999999999999929, 0.000000000000000000 ) ) ;
#18358 = AXIS2_PLACEMENT_3D ( 'NONE', #6683, #5013, #12398 ) ;
#18359 = CARTESIAN_POINT ( 'NONE',  ( -19.94028570965000213, -9.569631055272999731, 0.0004266524341263999969 ) ) ;
#18360 = CARTESIAN_POINT ( 'NONE',  ( 12.28779254565060519, -7.992768853820558128, -11.15614400032192144 ) ) ;
#18361 = LINE ( 'NONE', #23583, #13493 ) ;
#18362 = CARTESIAN_POINT ( 'NONE',  ( -22.85194746286182976, -7.255022703790015903, -7.682962849886891377 ) ) ;
#18363 = CARTESIAN_POINT ( 'NONE',  ( -2.145417483866896013, 27.78421022192531709, -0.3448129055962916301 ) ) ;
#18364 = COLOUR_RGB ( '', 0.40784314, 0.44705882, 0.49803922) ;
#18365 = CARTESIAN_POINT ( 'NONE',  ( 2.826365205286999860, 28.43750240009999786, 0.5047246425490000687 ) ) ;
#18366 = EDGE_CURVE ( 'NONE', #20885, #23589, #6475, .T. ) ;
#18367 = CARTESIAN_POINT ( 'NONE',  ( 1.888917822874810026, 30.66857564960811189, -1.051002523236465924 ) ) ;
#18368 = ORIENTED_EDGE ( 'NONE', *, *, #14010, .T. ) ;
#18369 = CARTESIAN_POINT ( 'NONE',  ( 4.423436775227599149, 14.62387349557263505, 4.241731953385504461 ) ) ;
#18370 = CARTESIAN_POINT ( 'NONE',  ( 1.539407619234959501, 24.77839267836325021, 1.461333290478949332 ) ) ;
#18371 = CARTESIAN_POINT ( 'NONE',  ( 6.095484411338158104, 14.38176773113363360, -0.6831047453619784049 ) ) ;
#18372 = CARTESIAN_POINT ( 'NONE',  ( 2.287373719275000106, 27.43021896306000329, 0.04491825056504000074 ) ) ;
#18373 = CARTESIAN_POINT ( 'NONE',  ( -2.122871095894375948, 30.87585552377906595, 0.07971169187474370921 ) ) ;
#18374 = CIRCLE ( 'NONE', #4459, 4.750000000000000000 ) ;
#18375 = CARTESIAN_POINT ( 'NONE',  ( 2.018676308209844894, 11.65591130541151088, 4.375244769163982639 ) ) ;
#18376 = VERTEX_POINT ( 'NONE', #895 ) ;
#18377 = CARTESIAN_POINT ( 'NONE',  ( -4.237782011582903685, 12.22811978868115190, -2.340022628918474457 ) ) ;
#18378 = EDGE_CURVE ( 'NONE', #5746, #19819, #13983, .T. ) ;
#18379 = CARTESIAN_POINT ( 'NONE',  ( -10.73781098442203330, 15.39563139958459104, 1.589574342470376100 ) ) ;
#18380 = CARTESIAN_POINT ( 'NONE',  ( 1.412335231500430277, 28.94512266248814925, -1.787330250453557090 ) ) ;
#18381 = ORIENTED_EDGE ( 'NONE', *, *, #4648, .F. ) ;
#18382 = FACE_OUTER_BOUND ( 'NONE', #20847, .T. ) ;
#18383 = CARTESIAN_POINT ( 'NONE',  ( -5.194121241700999647, 12.44999999995000017, 4.899969256345999539E-10 ) ) ;
#18384 = CARTESIAN_POINT ( 'NONE',  ( 17.69737658530999980, -0.08473977435852000917, -10.25642497589999991 ) ) ;
#18385 = CARTESIAN_POINT ( 'NONE',  ( 18.46827294453634849, 10.07514253733398490, -2.674013015929876946 ) ) ;
#18386 = CARTESIAN_POINT ( 'NONE',  ( 7.446152422707000618, 28.20096189432300093, 6.000000000000000000 ) ) ;
#18387 = CARTESIAN_POINT ( 'NONE',  ( 1.999533992831999729, 29.69566833366999958, 0.7922197204133999415 ) ) ;
#18388 = CARTESIAN_POINT ( 'NONE',  ( -12.50958960166000189, 6.524993957290000424, -6.187564705242000862 ) ) ;
#18389 = CARTESIAN_POINT ( 'NONE',  ( 13.50000000000000000, -9.107210294142168650, 3.887247416875642791 ) ) ;
#18390 = AXIS2_PLACEMENT_3D ( 'NONE', #9898, #21038, #13403 ) ;
#18391 = ORIENTED_EDGE ( 'NONE', *, *, #5373, .T. ) ;
#18392 = CARTESIAN_POINT ( 'NONE',  ( -2.434931691670786602, 28.83333333333333215, 0.6543697108982093891 ) ) ;
#18393 = CARTESIAN_POINT ( 'NONE',  ( 24.19673057186000165, 6.858943761402000128, 9.064940718355000371 ) ) ;
#18394 = EDGE_CURVE ( 'NONE', #12844, #19694, #11792, .T. ) ;
#18395 = CARTESIAN_POINT ( 'NONE',  ( -24.07222078679921040, 5.017431004176742704, 8.537427716843492220 ) ) ;
#18396 = DIRECTION ( 'NONE',  ( -0.5000000000000169864, 0.000000000000000000, 0.8660254037844289376 ) ) ;
#18397 = LINE ( 'NONE', #16804, #18410 ) ;
#18398 = CARTESIAN_POINT ( 'NONE',  ( -4.796084242829001809, 12.39410533642999468, 1.092145777077000890 ) ) ;
#18399 =( REPRESENTATION_RELATIONSHIP ('NONE','NONE', #13682, #8755 ) REPRESENTATION_RELATIONSHIP_WITH_TRANSFORMATION ( #16049 )SHAPE_REPRESENTATION_RELATIONSHIP( ) );
#18400 = CARTESIAN_POINT ( 'NONE',  ( -0.4160351173932703150, 29.22861210950169308, -2.119817327165559817 ) ) ;
#18401 = CARTESIAN_POINT ( 'NONE',  ( -20.80699594585999890, -9.665068862928000826, -5.402836533902000582 ) ) ;
#18402 = ORIENTED_EDGE ( 'NONE', *, *, #3722, .F. ) ;
#18403 = DIRECTION ( 'NONE',  ( 0.000000000000000000, 5.996561511235000638E-10, -1.000000000000000000 ) ) ;
#18404 = ORIENTED_EDGE ( 'NONE', *, *, #6748, .F. ) ;
#18405 = CARTESIAN_POINT ( 'NONE',  ( 1.092712698506000057, 24.81118861319000146, 1.864679196896000146 ) ) ;
#18406 = CARTESIAN_POINT ( 'NONE',  ( -1.259047450927242462, 28.13333333333332931, 2.184465970885648201 ) ) ;
#18407 = CIRCLE ( 'NONE', #21886, 4.750000000000000000 ) ;
#18408 = EDGE_CURVE ( 'NONE', #14395, #15392, #21462, .T. ) ;
#18409 = CARTESIAN_POINT ( 'NONE',  ( 12.12543434883977866, 5.255139125105725562, -12.50003690308978221 ) ) ;
#18410 = VECTOR ( 'NONE', #13177, 1000.000000000000000 ) ;
#18411 = CARTESIAN_POINT ( 'NONE',  ( -2.749999993363999806, 22.20000000663619844, 7.185653392336999782E-09 ) ) ;
#18412 = CARTESIAN_POINT ( 'NONE',  ( 0.000000000000000000, 24.50000000000000000, 0.000000000000000000 ) ) ;
#18413 = CARTESIAN_POINT ( 'NONE',  ( 14.51643908531000093, 10.16840836635999956, -0.3108424006793999994 ) ) ;
#18414 = VERTEX_POINT ( 'NONE', #15790 ) ;
#18415 = CYLINDRICAL_SURFACE ( 'NONE', #14313, 15.43375672974000068 ) ;
#18416 = CARTESIAN_POINT ( 'NONE',  ( -4.080056528100000079, 28.00000000000000000, 4.563746053395999702 ) ) ;
#18417 = EDGE_CURVE ( 'NONE', #7412, #13026, #13964, .T. ) ;
#18418 = DIRECTION ( 'NONE',  ( 0.000000000000000000, 1.000000000000000000, 0.000000000000000000 ) ) ;
#18419 = VERTEX_POINT ( 'NONE', #21132 ) ;
#18420 = CARTESIAN_POINT ( 'NONE',  ( -21.19117780174000032, -10.95007088059999845, 2.483471832359000153 ) ) ;
#18421 = CARTESIAN_POINT ( 'NONE',  ( -1.109476331411000105, 25.04810348418999766, -2.054679907054999699 ) ) ;
#18422 = CARTESIAN_POINT ( 'NONE',  ( 14.48754660397587024, 0.8598977260950438906, -10.31086185088971341 ) ) ;
#18423 = CARTESIAN_POINT ( 'NONE',  ( 25.72500000000000142, 0.000000000000000000, 0.000000000000000000 ) ) ;
#18424 = CARTESIAN_POINT ( 'NONE',  ( 22.54674094339000234, 7.224650810196000528, 8.638435146791000108 ) ) ;
#18425 = ADVANCED_FACE ( 'NONE', ( #4673 ), #15240, .F. ) ;
#18426 = CARTESIAN_POINT ( 'NONE',  ( -0.7614732458495000467, 28.54087351380000115, 2.105206779053000243 ) ) ;
#18427 = CARTESIAN_POINT ( 'NONE',  ( 14.07840962283755459, 5.123541359228647174, 7.439753567503393228 ) ) ;
#18428 = EDGE_CURVE ( 'NONE', #2392, #7244, #5598, .T. ) ;
#18429 = CARTESIAN_POINT ( 'NONE',  ( -2.125825771822000831, 11.86025111954001510, -4.338660460033000099 ) ) ;
#18430 = LINE ( 'NONE', #3198, #10649 ) ;
#18431 = ORIENTED_EDGE ( 'NONE', *, *, #23913, .T. ) ;
#18432 = CARTESIAN_POINT ( 'NONE',  ( -1.326172741988208337, 24.10416131130349271, -2.158080337669399551 ) ) ;
#18433 = CARTESIAN_POINT ( 'NONE',  ( 23.99062354302999722, 7.716878364870000340, -11.63397459621999985 ) ) ;
#18434 = VERTEX_POINT ( 'NONE', #19189 ) ;
#18435 = CARTESIAN_POINT ( 'NONE',  ( -16.03203743917331536, 1.189048994148058869, -9.082695391211098368 ) ) ;
#18436 = CARTESIAN_POINT ( 'NONE',  ( 1.119414263319356229, 30.77472232402685037, -1.944946624573452576 ) ) ;
#18437 = EDGE_CURVE ( 'NONE', #5630, #17905, #22693, .T. ) ;
#18438 = DIRECTION ( 'NONE',  ( 0.000000000000000000, 0.000000000000000000, 1.000000000000000000 ) ) ;
#18439 = AXIS2_PLACEMENT_3D ( 'NONE', #18122, #10852, #18234 ) ;
#18440 = ADVANCED_FACE ( 'NONE', ( #2479 ), #15627, .F. ) ;
#18441 = CARTESIAN_POINT ( 'NONE',  ( 15.74198797560999807, -10.51823260210000122, -3.385534472279999818 ) ) ;
#18442 = CARTESIAN_POINT ( 'NONE',  ( 0.3480762113532999691, 27.25000000000000000, 6.000000000000000000 ) ) ;
#18443 = CARTESIAN_POINT ( 'NONE',  ( 0.4339301335947999827, 26.20756359724000006, 2.429928970624000151 ) ) ;
#18444 = ORIENTED_EDGE ( 'NONE', *, *, #6981, .T. ) ;
#18445 = CIRCLE ( 'NONE', #4529, 4.625000000000000000 ) ;
#18446 = CARTESIAN_POINT ( 'NONE',  ( -11.11626113876999966, -12.56137170044999962, -8.591422195069000622 ) ) ;
#18447 = PLANE ( 'NONE',  #4750 ) ;
#18448 = CARTESIAN_POINT ( 'NONE',  ( -14.47125382252186299, -11.86037473473667170, -4.457180938895510813 ) ) ;
#18449 = ORIENTED_EDGE ( 'NONE', *, *, #763, .T. ) ;
#18450 = CARTESIAN_POINT ( 'NONE',  ( -3.783910185920449809, 14.59334639074173445, -4.817427536659290688 ) ) ;
#18451 = CARTESIAN_POINT ( 'NONE',  ( 19.85260141040004811, 5.075921885626229368, -9.207587878805371773 ) ) ;
#18452 = CARTESIAN_POINT ( 'NONE',  ( 60.61494135913342518, 37.01856778792605240, 2.673746900119611247 ) ) ;
#18453 = CARTESIAN_POINT ( 'NONE',  ( 16.01328496030753001, -8.173510217667363520, -6.363600821709828104 ) ) ;
#18454 = CARTESIAN_POINT ( 'NONE',  ( -16.42549441298000445, 9.777619552165999650, 5.164216230235000538 ) ) ;
#18455 = CARTESIAN_POINT ( 'NONE',  ( 1.534365737191000001, 29.70528949332000224, 1.770661353676000083 ) ) ;
#18456 = CONICAL_SURFACE ( 'NONE', #4542, 13.23032192316000000, 1.093540295016705466 ) ;
#18457 = CARTESIAN_POINT ( 'NONE',  ( -17.99241677431999875, 4.425129475628999387, -8.746809379632999537 ) ) ;
#18458 = CARTESIAN_POINT ( 'NONE',  ( 1.516020976517132635, 29.90463563117074131, -1.538576683859487204 ) ) ;
#18459 = VERTEX_POINT ( 'NONE', #13611 ) ;
#18460 = CARTESIAN_POINT ( 'NONE',  ( 2.087681966606000028, 25.60832866306000355, -0.3296552320861999563 ) ) ;
#18461 = CARTESIAN_POINT ( 'NONE',  ( 19.93039514411395885, 0.9077646897284779026, -10.46986812490325391 ) ) ;
#18462 = CIRCLE ( 'NONE', #656, 0.09999999855979024854 ) ;
#18463 = CARTESIAN_POINT ( 'NONE',  ( -0.9013079783759136987, 23.63028988911640127, -1.930365035980913468 ) ) ;
#18464 = ORIENTED_EDGE ( 'NONE', *, *, #10887, .T. ) ;
#18465 = DIRECTION ( 'NONE',  ( 0.000000000000000000, 1.000000000000000000, 0.000000000000000000 ) ) ;
#18466 = FACE_OUTER_BOUND ( 'NONE', #14365, .T. ) ;
#18467 = EDGE_CURVE ( 'NONE', #8416, #1912, #12560, .T. ) ;
#18468 = CARTESIAN_POINT ( 'NONE',  ( 1.417387361724000705, 11.51821284730998229, -4.666326094144003456 ) ) ;
#18469 = CARTESIAN_POINT ( 'NONE',  ( 13.47637625730999922, -3.210294990792000203, -8.544406387913998202 ) ) ;
#18470 = ORIENTED_EDGE ( 'NONE', *, *, #13997, .F. ) ;
#18471 = AXIS2_PLACEMENT_3D ( 'NONE', #14883, #22397, #16820 ) ;
#18472 = CARTESIAN_POINT ( 'NONE',  ( 0.000000000000000000, 22.19999999999999574, 0.000000000000000000 ) ) ;
#18473 = APPLICATION_PROTOCOL_DEFINITION ( 'draft international standard', 'automotive_design', 1998, #11751 ) ;
#18474 = CARTESIAN_POINT ( 'NONE',  ( 12.50000000000000000, -13.93375672974000068, 0.000000000000000000 ) ) ;
#18475 = B_SPLINE_SURFACE_WITH_KNOTS ( 'NONE', 3, 3, ( 
 ( #14645, #12603, #16807, #10908, #12722, #21919, #18521, #20116, #1693, #2046, #9082, #9436, #16454, #5451, #20228, #14872, #3632, #5221, #9319, #215, #7610, #7373, #16693, #18401, #1812, #22259, #14757, #5564, #12941, #20460, #11262, #21806, #3411, #5799, #18750 ),
 ( #9673, #19232, #9553, #21049, #20570, #10041, #6026, #13181, #17172, #13538, #17295, #696, #4223, #22618, #567, #16931, #19106, #819, #13413, #15345, #8103, #20813, #22735, #2160, #17053, #451, #15470, #22856, #2647, #7853, #6149, #334, #4463, #3984, #17425 ),
 ( #11617, #7737, #11378, #15104, #22498, #9907, #18987, #5907, #4340, #13293, #14988, #20692, #4100, #9787, #15220, #2397, #11852, #11731, #2517, #22384, #11497, #7973, #6270, #18874, #13653, #2280, #20934, #23339, #3016, #15702, #1062, #8464, #15832, #1315, #10528 ),
 ( #4958, #6517, #6876, #8337, #10157, #13774, #21174, #6755, #3259, #8703, #16068, #23220, #4831, #4588, #14148, #17543, #10402, #1192, #23094, #17912, #21543, #21301, #21418, #13902, #6635, #6390, #12460, #23464, #12342, #2771, #4714, #22975, #19734, #15947, #19366 ) ),
 .UNSPECIFIED., .F., .F., .F.,
 ( 4, 4 ),
 ( 4, 1, 1, 1, 1, 1, 1, 1, 1, 1, 1, 1, 1, 1, 1, 1, 1, 1, 1, 1, 1, 1, 1, 1, 1, 1, 1, 1, 1, 1, 1, 1, 4 ),
 ( -0.6000240009599999702, 1.600024000959999970 ),
 ( 0.1610006166028000174, 0.1877334400934000114, 0.2144662635840000053, 0.2411990870745999993, 0.2679319105651999933, 0.2946647340557999595, 0.3213975575463999812, 0.3481303810370000029, 0.3748632045276000246, 0.4015960280181999908, 0.4283288515088000126, 0.4550616749994000343, 0.4817944984900000005, 0.5085273219806000222, 0.5352601454711999329, 0.5619929689617000346, 0.5887257924522999453, 0.6154586159428999670, 0.6421914394334999887, 0.6689242629241000104, 0.6956570864147000322, 0.7223899099052999428, 0.7491227333958999646, 0.7758555568864999863, 0.8025883803771000080, 0.8293212038677000297, 0.8560540273582999404, 0.8827868508488999622, 0.9095196743394999839, 0.9362524978301000056, 0.9629853213207000273, 0.9897181448113000490, 1.016450968301999991 ),
 .UNSPECIFIED. ) ;
#18476 = ORIENTED_EDGE ( 'NONE', *, *, #18428, .T. ) ;
#18477 = CARTESIAN_POINT ( 'NONE',  ( 0.000000000000000000, 24.50000000000000000, 0.000000000000000000 ) ) ;
#18478 = CARTESIAN_POINT ( 'NONE',  ( -22.61826676953999993, 4.526472954474000332, 8.498838343196000622 ) ) ;
#18479 = CARTESIAN_POINT ( 'NONE',  ( 11.92450592358771999, -8.469720391588866804, -10.33010329016888029 ) ) ;
#18480 = CARTESIAN_POINT ( 'NONE',  ( -8.099999999999999645, 1.323843189878000027E-14, 0.000000000000000000 ) ) ;
#18481 = CARTESIAN_POINT ( 'NONE',  ( -18.13088126894000141, 9.136555860487012737, 0.000000000000000000 ) ) ;
#18482 = CARTESIAN_POINT ( 'NONE',  ( 1.165223649068083844, 26.45298450433979554, -2.066627348871238556 ) ) ;
#18483 = CARTESIAN_POINT ( 'NONE',  ( 15.69158333333333211, 8.837836392473214175, 2.374972199734133760 ) ) ;
#18484 = CARTESIAN_POINT ( 'NONE',  ( -6.058164523583997152, 16.51672836841997949, 0.9500184723446998269 ) ) ;
#18485 = CARTESIAN_POINT ( 'NONE',  ( 12.00000000000000000, 7.500000000000000000, 0.000000000000000000 ) ) ;
#18486 = ORIENTED_EDGE ( 'NONE', *, *, #11625, .T. ) ;
#18487 = CARTESIAN_POINT ( 'NONE',  ( -17.73266243917333185, 4.596313708240831630, -7.974420273544428284 ) ) ;
#18488 = CARTESIAN_POINT ( 'NONE',  ( 3.446647972078433764, 14.26578946693170558, 5.064530567705452846 ) ) ;
#18489 = CARTESIAN_POINT ( 'NONE',  ( 14.37123251481000530, 5.018772503670207108, 7.581327530252383262 ) ) ;
#18490 = AXIS2_PLACEMENT_3D ( 'NONE', #12520, #18091, #3440 ) ;
#18491 = CARTESIAN_POINT ( 'NONE',  ( -21.66177666636737342, 4.758819052736769528, 9.550088228515980049 ) ) ;
#18492 = CARTESIAN_POINT ( 'NONE',  ( -2.276798263289999902, 27.82021896306000031, -0.2242450566329000083 ) ) ;
#18493 = CARTESIAN_POINT ( 'NONE',  ( 1.871649831644675466, 11.63140178027804161, 4.440172657072205098 ) ) ;
#18494 = ORIENTED_EDGE ( 'NONE', *, *, #5783, .T. ) ;
#18495 = CONICAL_SURFACE ( 'NONE', #6102, 13.23032192316000000, 1.235249617460683957 ) ;
#18496 = CARTESIAN_POINT ( 'NONE',  ( -0.4068995525957177506, 11.48930230209881387, -4.795673420918372898 ) ) ;
#18497 = CARTESIAN_POINT ( 'NONE',  ( 23.99478584078000054, -6.383504859148000143, -12.40379814867000086 ) ) ;
#18498 = AXIS2_PLACEMENT_3D ( 'NONE', #2783, #23103, #6529 ) ;
#18499 = CARTESIAN_POINT ( 'NONE',  ( 0.1562663868984598969, 28.63946909753791914, 2.160009633825578756 ) ) ;
#18500 = VERTEX_POINT ( 'NONE', #11812 ) ;
#18501 = EDGE_CURVE ( 'NONE', #16087, #23589, #13312, .T. ) ;
#18502 = CARTESIAN_POINT ( 'NONE',  ( -16.52332910583999848, -9.095302903661998783, 0.000000000000000000 ) ) ;
#18503 = AXIS2_PLACEMENT_3D ( 'NONE', #16346, #23734, #5336 ) ;
#18504 = CARTESIAN_POINT ( 'NONE',  ( 12.65175158531000044, 9.909822556590000886, -2.072115565883000166 ) ) ;
#18505 = CARTESIAN_POINT ( 'NONE',  ( 18.29206332576804073, 6.690873865058084569, -7.988726941084996369 ) ) ;
#18506 = CARTESIAN_POINT ( 'NONE',  ( 0.3272492347489454056, 29.25086340285666608, 2.499999999999998668 ) ) ;
#18507 = CARTESIAN_POINT ( 'NONE',  ( 0.3299503294897000449, 29.56330889271999851, 2.125295521557999834 ) ) ;
#18508 = DIRECTION ( 'NONE',  ( 0.000000000000000000, -1.000000000000000000, 0.000000000000000000 ) ) ;
#18509 = DIRECTION ( 'NONE',  ( 0.000000000000000000, -1.000000000000000000, 0.000000000000000000 ) ) ;
#18510 = ORIENTED_EDGE ( 'NONE', *, *, #7923, .T. ) ;
#18511 = CARTESIAN_POINT ( 'NONE',  ( -24.17970357211641286, 12.87935348060952379, 2.692294542479934716 ) ) ;
#18512 = CARTESIAN_POINT ( 'NONE',  ( 21.89509224385000152, 8.147067418188999710, -7.836651225645998586 ) ) ;
#18513 = EDGE_CURVE ( 'NONE', #22006, #1172, #2104, .T. ) ;
#18514 = CARTESIAN_POINT ( 'NONE',  ( -24.36228659953834352, 8.887038971774549267, -5.014620418582080852 ) ) ;
#18515 = EDGE_LOOP ( 'NONE', ( #4321, #11188, #16497, #16266, #10077 ) ) ;
#18516 = CARTESIAN_POINT ( 'NONE',  ( 13.52795396126032479, -5.741355442642295692, 8.603735498112436986 ) ) ;
#18517 = DIRECTION ( 'NONE',  ( 0.000000000000000000, 1.000000000000000000, 0.000000000000000000 ) ) ;
#18518 = MECHANICAL_DESIGN_GEOMETRIC_PRESENTATION_REPRESENTATION (  '', ( #23553 ), #20456 ) ;
#18519 = CARTESIAN_POINT ( 'NONE',  ( -4.727635250208997775, 12.45903567298001668, 0.7257861805102000519 ) ) ;
#18520 = CARTESIAN_POINT ( 'NONE',  ( 1.438533966298229494, 29.11160131773634774, -1.622102280252738060 ) ) ;
#18521 = CARTESIAN_POINT ( 'NONE',  ( -23.64743322413000115, 11.09837689733000055, 1.069113796759999957 ) ) ;
#18522 = ORIENTED_EDGE ( 'NONE', *, *, #1261, .T. ) ;
#18523 = DIRECTION ( 'NONE',  ( 0.000000000000000000, 1.000000000000000000, -6.254606381427991854E-11 ) ) ;
#18524 = CIRCLE ( 'NONE', #16183, 7.100000000000000533 ) ;
#18525 = ORIENTED_EDGE ( 'NONE', *, *, #18603, .T. ) ;
#18526 = CARTESIAN_POINT ( 'NONE',  ( 0.3718092809970000023, 24.42893128708999839, -2.323663357635999738 ) ) ;
#18527 = CARTESIAN_POINT ( 'NONE',  ( 5.504749613137996711, 13.91273307856000940, 3.018176302422998614 ) ) ;
#18528 = CARTESIAN_POINT ( 'NONE',  ( -8.099999999999999645, 1.323843189878000027E-14, 0.000000000000000000 ) ) ;
#18529 = CARTESIAN_POINT ( 'NONE',  ( -16.97092920454666753, -7.957437029153473951, 4.586234609216395697 ) ) ;
#18530 = SPHERICAL_SURFACE ( 'NONE', #9551, 12.50000000000000000 ) ;
#18531 = CARTESIAN_POINT ( 'NONE',  ( 15.72300158530999958, -5.453124986814999353, -8.625711720232999369 ) ) ;
#18532 = VECTOR ( 'NONE', #4125, 1000.000000000000227 ) ;
#18533 = EDGE_CURVE ( 'NONE', #12632, #11620, #9331, .T. ) ;
#18534 =( NAMED_UNIT ( * ) SI_UNIT ( $, .STERADIAN. ) SOLID_ANGLE_UNIT ( ) );
#18535 = ORIENTED_EDGE ( 'NONE', *, *, #19795, .F. ) ;
#18536 = FACE_OUTER_BOUND ( 'NONE', #23036, .T. ) ;
#18537 = AXIS2_PLACEMENT_3D ( 'NONE', #846, #8249, #15616 ) ;
#18538 = CARTESIAN_POINT ( 'NONE',  ( -10.34021276376999943, 1.351277883783999990E-14, 0.000000000000000000 ) ) ;
#18539 = CARTESIAN_POINT ( 'NONE',  ( -6.000000000000000000, 24.99999999999999645, 1.000000000000000000 ) ) ;
#18540 = ORIENTED_EDGE ( 'NONE', *, *, #8687, .F. ) ;
#18541 = CARTESIAN_POINT ( 'NONE',  ( -19.64887718127000227, -4.424839147307999987, 10.27402513662999972 ) ) ;
#18542 = CARTESIAN_POINT ( 'NONE',  ( -2.212662158434000048, 24.34365122578000040, -0.7461725103679001103 ) ) ;
#18543 = CARTESIAN_POINT ( 'NONE',  ( 14.39581696055360815, -2.328303387492436372, -10.05895166234070714 ) ) ;
#18544 = CONICAL_SURFACE ( 'NONE', #5395, 4.309401076758999416, 1.119376321708719590 ) ;
#18545 = CARTESIAN_POINT ( 'NONE',  ( -18.36922087121333647, -5.618509400322853509, -7.311181514368041867 ) ) ;
#18546 = CARTESIAN_POINT ( 'NONE',  ( 22.17964701745000156, 10.37524365059999809, -4.352655460828000145 ) ) ;
#18547 = CARTESIAN_POINT ( 'NONE',  ( 1.488049260313999866, 30.15885213760000028, 2.074625148294999999 ) ) ;
#18548 = EDGE_CURVE ( 'NONE', #2983, #1045, #548, .T. ) ;
#18549 = CARTESIAN_POINT ( 'NONE',  ( 13.70789982098004423, 8.571058519759501948, -2.817337828859955096 ) ) ;
#18550 = CARTESIAN_POINT ( 'NONE',  ( -6.500384775316716990, 15.46782671400865539, -1.463283840608048614 ) ) ;
#18551 = B_SPLINE_CURVE_WITH_KNOTS ( 'NONE', 3,
 ( #15202, #18730, #2139, #9529, #11113, #5539, #22479, #4198, #22362, #5889 ),
 .UNSPECIFIED., .F., .F.,
 ( 4, 1, 1, 2, 2, 4 ),
 ( 0.000000000000000000, 0.2499999999999996669, 0.3749999999999997224, 0.4374999999999996114, 0.4999999999999995559, 1.000000000000000000 ),
 .UNSPECIFIED. ) ;
#18552 = AXIS2_PLACEMENT_3D ( 'NONE', #16970, #11174, #4016 ) ;
#18553 = CARTESIAN_POINT ( 'NONE',  ( 18.85055757573999813, 0.1142443464370000022, 10.79806225559999966 ) ) ;
#18554 = ORIENTED_EDGE ( 'NONE', *, *, #10737, .T. ) ;
#18555 = CARTESIAN_POINT ( 'NONE',  ( 2.369722497171532272, 23.91240411898208151, -0.5226290486314587591 ) ) ;
#18556 = TOROIDAL_SURFACE ( 'NONE', #5024, 10.69999999999999929, 0.8000000000000000444 ) ;
#18557 = B_SPLINE_CURVE_WITH_KNOTS ( 'NONE', 3,
 ( #4047, #1757, #400, #7318, #12885, #10096, #17118, #2345, #2836, #20880, #20993, #19173, #15529, #11677, #7918, #19050 ),
 .UNSPECIFIED., .F., .F.,
 ( 4, 2, 2, 2, 2, 2, 2, 4 ),
 ( 0.0007950867507350306432, 0.001248881430381147684, 0.001702676110027264832, 0.002156470789673382415, 0.002610265469319499564, 0.003517854828611732994, 0.003971649508257850576, 0.004425444187903967291 ),
 .UNSPECIFIED. ) ;
#18558 = EDGE_CURVE ( 'NONE', #2559, #12315, #21499, .T. ) ;
#18559 = ORIENTED_EDGE ( 'NONE', *, *, #23708, .F. ) ;
#18560 = DIRECTION ( 'NONE',  ( 0.000000000000000000, 1.000000000000000000, 0.000000000000000000 ) ) ;
#18561 = FACE_OUTER_BOUND ( 'NONE', #3396, .T. ) ;
#18562 = CARTESIAN_POINT ( 'NONE',  ( 22.09812270046333182, -8.072307342008256725, 4.652732286360434344 ) ) ;
#18563 = CARTESIAN_POINT ( 'NONE',  ( 13.57657720147000013, -6.781973559127000506, 8.648568256107001417 ) ) ;
#18564 = CARTESIAN_POINT ( 'NONE',  ( -1.989999999999999991, 9.799994897958001161, 7.500000000000000000 ) ) ;
#18565 = EDGE_CURVE ( 'NONE', #6719, #11336, #10238, .T. ) ;
#18566 = CARTESIAN_POINT ( 'NONE',  ( 2.669209039122999894, 27.07712896666999924, 0.05241653317053000111 ) ) ;
#18567 = ORIENTED_EDGE ( 'NONE', *, *, #11923, .T. ) ;
#18568 = ORIENTED_EDGE ( 'NONE', *, *, #22088, .F. ) ;
#18569 = CARTESIAN_POINT ( 'NONE',  ( -10.40350363876999928, 13.74367368368000086, 6.535443979581000207 ) ) ;
#18570 = FACE_OUTER_BOUND ( 'NONE', #17855, .T. ) ;
#18571 = CARTESIAN_POINT ( 'NONE',  ( -14.49284522991462509, -10.30702784337245248, -7.147655011466097719 ) ) ;
#18572 = EDGE_LOOP ( 'NONE', ( #6302, #15252, #16082, #6647, #15032, #14674, #18049, #15174, #12617, #22874, #20733, #380, #2314 ) ) ;
#18573 = CARTESIAN_POINT ( 'NONE',  ( -14.49999963946489423, 11.08494587601020065, 5.800314632267468795 ) ) ;
#18574 = FACE_BOUND ( 'NONE', #7868, .T. ) ;
#18575 = CARTESIAN_POINT ( 'NONE',  ( 6.242982157972016388, 13.64690610122263514, 1.860940423144956446 ) ) ;
#18576 = CARTESIAN_POINT ( 'NONE',  ( 16.01456160276670104, -8.144906968459116214, -6.400242916633066770 ) ) ;
#18577 = CARTESIAN_POINT ( 'NONE',  ( -18.55941247522000381, 11.04350775505000115, -1.268070264779000089 ) ) ;
#18578 = CARTESIAN_POINT ( 'NONE',  ( -2.187619468058000116, 29.43588321332000035, 0.05437783349231000568 ) ) ;
#18579 = EDGE_CURVE ( 'NONE', #8876, #2459, #2372, .T. ) ;
#18580 = B_SPLINE_CURVE_WITH_KNOTS ( 'NONE', 3,
 ( #22980, #19111, #4467, #4230, #15351, #6157, #4105, #6394, #7858, #13542, #20697, #2523, #944, #6030, #19369, #2286, #8341, #9912 ),
 .UNSPECIFIED., .F., .F.,
 ( 4, 2, 2, 2, 2, 2, 2, 2, 4 ),
 ( 0.000000000000000000, 0.1250000000000000555, 0.2500000000000000555, 0.3750000000000000000, 0.4999999999999999445, 0.6249999999999998890, 0.7500000000000000000, 0.8750000000000000000, 1.000000000000000000 ),
 .UNSPECIFIED. ) ;
#18581 = CARTESIAN_POINT ( 'NONE',  ( -19.08958467661999947, -10.87501988123999830, 0.7812661330421999395 ) ) ;
#18582 = CARTESIAN_POINT ( 'NONE',  ( 1.222085875088660512, 29.68033221944324040, 1.780880044240042537 ) ) ;
#18583 = ORIENTED_EDGE ( 'NONE', *, *, #7789, .F. ) ;
#18584 = CARTESIAN_POINT ( 'NONE',  ( -2.150969990163999590, 23.76339666646000026, -0.9104165138074999941 ) ) ;
#18585 = CARTESIAN_POINT ( 'NONE',  ( 21.71791831486828173, -0.02456864104712422336, -10.71023399046199209 ) ) ;
#18586 = DIRECTION ( 'NONE',  ( -0.1671082301074949539, 0.9859385576344705804, 0.000000000000000000 ) ) ;
#18587 = ORIENTED_EDGE ( 'NONE', *, *, #1089, .T. ) ;
#18588 = DIRECTION ( 'NONE',  ( 0.000000000000000000, 0.000000000000000000, 1.000000000000000000 ) ) ;
#18589 = CARTESIAN_POINT ( 'NONE',  ( -4.823557208340003122, 13.17411124896998764, 5.974450474228996555 ) ) ;
#18590 = LINE ( 'NONE', #5862, #13022 ) ;
#18591 = ADVANCED_FACE ( 'NONE', ( #20161 ), #5043, .F. ) ;
#18592 = CARTESIAN_POINT ( 'NONE',  ( 18.43875142131000189, -2.600393254974000090, 9.414598814742999977 ) ) ;
#18593 = ADVANCED_FACE ( 'NONE', ( #8660 ), #19058, .F. ) ;
#18594 = EDGE_LOOP ( 'NONE', ( #5859, #21003, #19653 ) ) ;
#18595 = LINE ( 'NONE', #3587, #7909 ) ;
#18596 = CARTESIAN_POINT ( 'NONE',  ( -14.47826287373678156, 1.813202974803316048, -12.50000251924343608 ) ) ;
#18597 = EDGE_LOOP ( 'NONE', ( #2835, #1592, #13592, #19542 ) ) ;
#18598 = CARTESIAN_POINT ( 'NONE',  ( -15.64822087121333460, 5.575597924126876492, 7.255343799257086168 ) ) ;
#18599 = CARTESIAN_POINT ( 'NONE',  ( -2.587409587117002641, 11.93419056235999953, 3.993438532374998573 ) ) ;
#18600 = AXIS2_PLACEMENT_3D ( 'NONE', #9792, #12579, #12104 ) ;
#18601 = DIRECTION ( 'NONE',  ( 1.000000000000000000, 0.000000000000000000, 0.000000000000000000 ) ) ;
#18602 = EDGE_CURVE ( 'NONE', #18819, #14273, #1732, .T. ) ;
#18603 = EDGE_CURVE ( 'NONE', #14220, #14865, #11667, .T. ) ;
#18604 = CARTESIAN_POINT ( 'NONE',  ( -20.76740227730209654, 1.886003063178867123, -10.34259919642779657 ) ) ;
#18605 = DIRECTION ( 'NONE',  ( 0.7071067811865474617, -0.7071067811865474617, 0.000000000000000000 ) ) ;
#18606 = CARTESIAN_POINT ( 'NONE',  ( -2.500000000000000000, 26.63419673618999894, 0.000000000000000000 ) ) ;
#18607 = CARTESIAN_POINT ( 'NONE',  ( -5.966878999860996124, 15.10316773259998868, 2.678439550780997713 ) ) ;
#18608 = CARTESIAN_POINT ( 'NONE',  ( -0.6269526792712883934, 30.36641892158466050, 2.067003944720025466 ) ) ;
#18609 = ORIENTED_EDGE ( 'NONE', *, *, #10158, .T. ) ;
#18610 = CARTESIAN_POINT ( 'NONE',  ( -17.43032910583999850, 9.118578311265999048, 0.000000000000000000 ) ) ;
#18611 = CARTESIAN_POINT ( 'NONE',  ( 22.30022314420000029, -9.218578328389000376, -3.456323596348999772 ) ) ;
#18612 = CARTESIAN_POINT ( 'NONE',  ( 14.18456538144702961, 8.569177250714071548, 3.026341649409048706 ) ) ;
#18613 = CARTESIAN_POINT ( 'NONE',  ( -23.67000479291073489, 9.608364060292810649, 4.444627409576130006 ) ) ;
#18614 = DIRECTION ( 'NONE',  ( 1.000000000000000000, 0.000000000000000000, 0.000000000000000000 ) ) ;
#18615 = CARTESIAN_POINT ( 'NONE',  ( 22.66677564524435340, 35.31760589360354885, -6.000000000000000000 ) ) ;
#18616 = CARTESIAN_POINT ( 'NONE',  ( 2.176439727641916289, 11.68391463016446963, 4.299875751357343567 ) ) ;
#18617 = ORIENTED_EDGE ( 'NONE', *, *, #9231, .F. ) ;
#18618 = CARTESIAN_POINT ( 'NONE',  ( -3.421692785168691575, 11.97394591298616007, -3.409861883590250109 ) ) ;
#18619 = CARTESIAN_POINT ( 'NONE',  ( -11.00000000000000000, 10.50000000000000000, 0.000000000000000000 ) ) ;
#18620 = DIRECTION ( 'NONE',  ( -1.000000000000000000, 0.000000000000000000, 0.000000000000000000 ) ) ;
#18621 = ORIENTED_EDGE ( 'NONE', *, *, #8989, .F. ) ;
#18622 = CARTESIAN_POINT ( 'NONE',  ( -1.775821082844895482, 26.49941889561072017, 1.759684967125137556 ) ) ;
#18623 = CARTESIAN_POINT ( 'NONE',  ( 11.63812642131000175, -9.225545160481999574, -2.612645831888999570 ) ) ;
#18624 = CARTESIAN_POINT ( 'NONE',  ( 18.39061514238058237, 8.952924735988446514, -5.333109133230360399 ) ) ;
#18625 = CARTESIAN_POINT ( 'NONE',  ( -0.3272492347489284192, 29.21753006952332754, 2.500000000000001332 ) ) ;
#18626 = CARTESIAN_POINT ( 'NONE',  ( 0.7229397994487999357, 29.10005084940000231, -2.025612581347999708 ) ) ;
#18627 = CARTESIAN_POINT ( 'NONE',  ( 16.27546080085999947, 2.142700662188999683, -11.17012464664999882 ) ) ;
#18628 = CARTESIAN_POINT ( 'NONE',  ( 13.50000000000000000, -4.002954420673999536, -8.080569262580000967 ) ) ;
#18629 = ORIENTED_EDGE ( 'NONE', *, *, #2886, .F. ) ;
#18630 = CARTESIAN_POINT ( 'NONE',  ( -11.00000000000000000, 1.359357947053999856E-14, 0.000000000000000000 ) ) ;
#18631 = CARTESIAN_POINT ( 'NONE',  ( 20.83279763092000181, -2.973987989840999990, 10.87602257598999955 ) ) ;
#18632 = VECTOR ( 'NONE', #14372, 1000.000000000000000 ) ;
#18633 = DIRECTION ( 'NONE',  ( -0.7071067811865462405, -0.7071067811865462405, -6.203608861676411764E-08 ) ) ;
#18634 = VERTEX_POINT ( 'NONE', #23388 ) ;
#18635 = CARTESIAN_POINT ( 'NONE',  ( 0.000000000000000000, 22.10000000618969906, 0.000000000000000000 ) ) ;
#18636 = DIRECTION ( 'NONE',  ( 0.000000000000000000, -1.000000000000000000, 0.000000000000000000 ) ) ;
#18637 = B_SPLINE_CURVE_WITH_KNOTS ( 'NONE', 3,
 ( #4066, #11460, #15189, #19069, #15072, #14950, #22586, #419, #18836, #7818, #2484, #20542, #22467, #5764, #20777, #9873, #11580, #15434 ),
 .UNSPECIFIED., .F., .F.,
 ( 4, 2, 2, 2, 2, 2, 2, 2, 4 ),
 ( 0.000000000000000000, 0.1250000000000000555, 0.2500000000000000555, 0.3750000000000000555, 0.5000000000000000000, 0.6249999999999998890, 0.7499999999999998890, 0.8749999999999998890, 1.000000000000000000 ),
 .UNSPECIFIED. ) ;
#18638 = CARTESIAN_POINT ( 'NONE',  ( 4.911758408288000588, 12.43820144620001145, -0.1548390653590999422 ) ) ;
#18639 = CARTESIAN_POINT ( 'NONE',  ( -1.368941726107665957, 29.29130111891828037, -1.671115392335038363 ) ) ;
#18640 = CARTESIAN_POINT ( 'NONE',  ( 0.000000000000000000, 29.85000000000000142, 0.000000000000000000 ) ) ;
#18641 = ORIENTED_EDGE ( 'NONE', *, *, #22278, .F. ) ;
#18642 = DIRECTION ( 'NONE',  ( 0.000000000000000000, -1.000000000000000000, 0.000000000000000000 ) ) ;
#18643 = ORIENTED_EDGE ( 'NONE', *, *, #9544, .T. ) ;
#18644 = CARTESIAN_POINT ( 'NONE',  ( -2.344138058790000034, 24.63794212566000041, -0.2065679117753000116 ) ) ;
#18645 = CARTESIAN_POINT ( 'NONE',  ( -1.536366799937282090, 28.11666666666666714, 1.999167105995454552 ) ) ;
#18646 = DIRECTION ( 'NONE',  ( 0.000000000000000000, 0.000000000000000000, -1.000000000000000000 ) ) ;
#18647 = DIRECTION ( 'NONE',  ( 1.000000000000000000, 0.000000000000000000, 0.000000000000000000 ) ) ;
#18648 = DIRECTION ( 'NONE',  ( 0.000000000000000000, 1.000000000000000000, 0.000000000000000000 ) ) ;
#18649 = DIRECTION ( 'NONE',  ( -1.000000000000000000, 0.000000000000000000, 0.000000000000000000 ) ) ;
#18650 = CARTESIAN_POINT ( 'NONE',  ( 13.77506424931000240, -10.16002631551000057, 3.235559929811000046 ) ) ;
#18651 = CARTESIAN_POINT ( 'NONE',  ( -18.84569624743000205, -10.33415972889999956, 0.7423446255362999846 ) ) ;
#18652 = AXIS2_PLACEMENT_3D ( 'NONE', #3562, #6827, #18332 ) ;
#18653 = CARTESIAN_POINT ( 'NONE',  ( 4.000000000000000888, 29.96241504948190482, 0.8002143650531877705 ) ) ;
#18654 = CARTESIAN_POINT ( 'NONE',  ( -14.45561360439974585, 2.584657965300122928, 12.49996445837907544 ) ) ;
#18655 = EDGE_LOOP ( 'NONE', ( #4808, #18235, #3694, #15164 ) ) ;
#18656 = CARTESIAN_POINT ( 'NONE',  ( -20.16297738808999895, 10.98403905672000036, 2.189746316398999859 ) ) ;
#18657 = CARTESIAN_POINT ( 'NONE',  ( 2.287833579909999582, 23.95940453936999859, 0.4674021866452000018 ) ) ;
#18658 = CARTESIAN_POINT ( 'NONE',  ( 13.93008789665596225, -9.927308807215476705, 2.819245968838537397 ) ) ;
#18659 = CYLINDRICAL_SURFACE ( 'NONE', #13329, 6.125000000000000000 ) ;
#18660 = CARTESIAN_POINT ( 'NONE',  ( 23.13430719836999927, -10.85154302445999974, -3.070125849493000381 ) ) ;
#18661 = CARTESIAN_POINT ( 'NONE',  ( 1.647802091131999935, 29.36895439600999680, 1.950156003153999951 ) ) ;
#18662 = CARTESIAN_POINT ( 'NONE',  ( 13.77521226315460723, 8.994996949847150702, -0.8114643769208054191 ) ) ;
#18663 = CARTESIAN_POINT ( 'NONE',  ( -6.383654667732219679, 15.56864394822520659, -1.329852007301480565 ) ) ;
#18664 = CARTESIAN_POINT ( 'NONE',  ( 0.000000000000000000, 24.80000000000000426, -4.618802153517000519 ) ) ;
#18665 = ADVANCED_FACE ( 'NONE', ( #10691 ), #16026, .T. ) ;
#18666 = CARTESIAN_POINT ( 'NONE',  ( 24.00391580400000180, 9.718215813663000802, 6.146681693640999811 ) ) ;
#18667 = ORIENTED_EDGE ( 'NONE', *, *, #18962, .T. ) ;
#18668 = AXIS2_PLACEMENT_3D ( 'NONE', #4760, #2940, #4346 ) ;
#18669 = CARTESIAN_POINT ( 'NONE',  ( 11.92450592357671901, -13.18099206878370921, 2.169941377000833338 ) ) ;
#18670 = EDGE_LOOP ( 'NONE', ( #8133, #7872, #3352, #23022 ) ) ;
#18671 = PRODUCT_DEFINITION_SHAPE ( 'NONE', 'NONE',  #116 ) ;
#18672 = DIRECTION ( 'NONE',  ( 0.000000000000000000, 1.000000000000000000, 0.000000000000000000 ) ) ;
#18673 = CARTESIAN_POINT ( 'NONE',  ( -19.10482910584000038, 9.161549281532014533, 0.000000000000000000 ) ) ;
#18674 = DIRECTION ( 'NONE',  ( 0.000000000000000000, -1.000000000000000000, 0.000000000000000000 ) ) ;
#18675 = CARTESIAN_POINT ( 'NONE',  ( 17.33221675526000283, -6.256935606695999574, 9.160251492536000129 ) ) ;
#18676 = CARTESIAN_POINT ( 'NONE',  ( -24.50000000000000000, -7.216878364870000340, 12.50000000000000000 ) ) ;
#18677 = CARTESIAN_POINT ( 'NONE',  ( -1.371352433351999744, 26.11006359723999992, 2.052373795670999979 ) ) ;
#18678 = EDGE_CURVE ( 'NONE', #9388, #8104, #19529, .T. ) ;
#18679 = EDGE_LOOP ( 'NONE', ( #20858, #857, #19394 ) ) ;
#18680 = ORIENTED_EDGE ( 'NONE', *, *, #10699, .F. ) ;
#18681 = CARTESIAN_POINT ( 'NONE',  ( -2.500000000000000000, 27.43419673618999965, 0.000000000000000000 ) ) ;
#18682 = LINE ( 'NONE', #15036, #8217 ) ;
#18683 = PLANE ( 'NONE',  #4791 ) ;
#18684 = ORIENTED_EDGE ( 'NONE', *, *, #18884, .F. ) ;
#18685 = CARTESIAN_POINT ( 'NONE',  ( 19.88366666666665949, -5.551639645582684857, 7.389795051981888463 ) ) ;
#18686 = CARTESIAN_POINT ( 'NONE',  ( 20.47308103379664956, -9.196661322686781048, -1.203713204382315327 ) ) ;
#18687 = DIRECTION ( 'NONE',  ( 0.000000000000000000, -1.000000000000000000, 0.000000000000000000 ) ) ;
#18688 = CARTESIAN_POINT ( 'NONE',  ( 15.93519615271878465, -9.616653625581596643, -3.849179279724161962 ) ) ;
#18689 = CARTESIAN_POINT ( 'NONE',  ( -19.31610745349000169, -11.07881103579000026, 1.129852276557000046 ) ) ;
#18690 = CARTESIAN_POINT ( 'NONE',  ( -2.353996515996000127, 30.01643588093000048, -0.1022769623496000008 ) ) ;
#18691 = CARTESIAN_POINT ( 'NONE',  ( -12.79254388956000099, 9.568035197138000214, -2.460455418527999871 ) ) ;
#18692 = EDGE_CURVE ( 'NONE', #15019, #14560, #21481, .T. ) ;
#18693 = CARTESIAN_POINT ( 'NONE',  ( -0.07238424743993485122, 29.59961443721505603, 2.158644815808733686 ) ) ;
#18694 = CARTESIAN_POINT ( 'NONE',  ( 2.087036767532999715, 24.27032282765000204, -0.6349553063932998898 ) ) ;
#18695 = CARTESIAN_POINT ( 'NONE',  ( -24.50000000000001066, -7.686026772365445403, -7.276726432132435640 ) ) ;
#18696 = CARTESIAN_POINT ( 'NONE',  ( -18.54343818302843516, 10.45866049467905512, 0.2745342069438318489 ) ) ;
#18697 = ORIENTED_EDGE ( 'NONE', *, *, #7068, .F. ) ;
#18698 = CARTESIAN_POINT ( 'NONE',  ( 24.34804274388863377, -3.330488627411554159, 12.49999999999999467 ) ) ;
#18699 = CARTESIAN_POINT ( 'NONE',  ( -2.000000000000000000, 26.50000000000000355, 3.464101615137999968 ) ) ;
#18700 = CARTESIAN_POINT ( 'NONE',  ( 18.51344355829000321, -6.966878364870000340, -12.06698729810999993 ) ) ;
#18701 = ADVANCED_FACE ( 'NONE', ( #8521 ), #21942, .T. ) ;
#18702 = CARTESIAN_POINT ( 'NONE',  ( 15.12168875731000028, -7.425874990359000449, -5.381511109182000041 ) ) ;
#18703 = ORIENTED_EDGE ( 'NONE', *, *, #20897, .T. ) ;
#18704 = CARTESIAN_POINT ( 'NONE',  ( -5.067526505253444391, 15.91328937823097789, 3.440358843088985097 ) ) ;
#18705 = LINE ( 'NONE', #9980, #21022 ) ;
#18706 = AXIS2_PLACEMENT_3D ( 'NONE', #1540, #11089, #14713 ) ;
#18707 = ORIENTED_EDGE ( 'NONE', *, *, #23593, .F. ) ;
#18708 = CARTESIAN_POINT ( 'NONE',  ( -14.25243324638999809, 7.716878364870000340, -11.63397459621999985 ) ) ;
#18709 = CARTESIAN_POINT ( 'NONE',  ( -4.247598233711002536, 12.43461358834999153, 2.282855730625001467 ) ) ;
#18710 = CARTESIAN_POINT ( 'NONE',  ( 11.99999999999999467, -3.013426419913816101, -9.057261035705595376 ) ) ;
#18711 = CARTESIAN_POINT ( 'NONE',  ( -14.29262089642102218, 7.983102671798921079, -11.17286057040529990 ) ) ;
#18712 = CARTESIAN_POINT ( 'NONE',  ( -4.357829670976999026, 15.67924589997999085, -4.374970551269004027 ) ) ;
#18713 = CARTESIAN_POINT ( 'NONE',  ( -23.74228231688656976, 8.693394395448456762E-05, -9.522797051439189531 ) ) ;
#18715 = AXIS2_PLACEMENT_3D ( 'NONE', #7775, #15141, #22538 ) ;
#18714 = CARTESIAN_POINT ( 'NONE',  ( 23.41677564524290744, 35.51856778792605240, -6.000000000000000000 ) ) ;
#18716 = ADVANCED_FACE ( 'NONE', ( #8994 ), #22599, .F. ) ;
#18717 = CARTESIAN_POINT ( 'NONE',  ( 0.3837787240339659012, 30.42650728909961444, 2.125527850226935023 ) ) ;
#18718 = ORIENTED_EDGE ( 'NONE', *, *, #21965, .T. ) ;
#18719 = EDGE_CURVE ( 'NONE', #14865, #611, #12509, .T. ) ;
#18720 = CARTESIAN_POINT ( 'NONE',  ( 24.41412816595000024, -8.463997690975000765, -5.186418078094000350 ) ) ;
#18721 = DIRECTION ( 'NONE',  ( 0.7071067811865474617, -0.7071067811865474617, -2.031299026805133754E-12 ) ) ;
#18722 = LINE ( 'NONE', #6115, #15323 ) ;
#18723 = CARTESIAN_POINT ( 'NONE',  ( -22.51862066702934939, -3.086810711953226427, -10.23562687710141894 ) ) ;
#18724 = CARTESIAN_POINT ( 'NONE',  ( -2.239169049547999890, 26.01614211382000263, 0.4912911496346999418 ) ) ;
#18725 = AXIS2_PLACEMENT_3D ( 'NONE', #10625, #16756, #5514 ) ;
#18726 = CARTESIAN_POINT ( 'NONE',  ( 12.52688711657000020, -6.216878364870000340, 12.50000000000000000 ) ) ;
#18727 = VERTEX_POINT ( 'NONE', #4883 ) ;
#18728 = CARTESIAN_POINT ( 'NONE',  ( -3.409519937314366977, 11.97052822634232605, -3.421840553652563788 ) ) ;
#18729 = EDGE_CURVE ( 'NONE', #12346, #1991, #21843, .T. ) ;
#18730 = CARTESIAN_POINT ( 'NONE',  ( -2.160826008357634720, 29.99999999999999645, 3.371248675920325510 ) ) ;
#18731 = EDGE_CURVE ( 'NONE', #259, #44, #940, .T. ) ;
#18732 = CONICAL_SURFACE ( 'NONE', #7135, 4.309401076758999416, 1.119376321708719590 ) ;
#18733 = DIRECTION ( 'NONE',  ( -1.000000000000000000, 0.000000000000000000, 0.000000000000000000 ) ) ;
#18734 = ORIENTED_EDGE ( 'NONE', *, *, #16113, .T. ) ;
#18735 = DIRECTION ( 'NONE',  ( 0.000000000000000000, 1.000000000000000000, 0.000000000000000000 ) ) ;
#18736 = CARTESIAN_POINT ( 'NONE',  ( 18.02643908530999894, 9.290813243320000581, -4.365746228316999655 ) ) ;
#18737 = DIRECTION ( 'NONE',  ( 0.000000000000000000, -0.5000000000000169864, 0.8660254037844288266 ) ) ;
#18738 = CARTESIAN_POINT ( 'NONE',  ( 22.87199999999999989, 9.258222311379999070, 0.000000000000000000 ) ) ;
#18739 = CARTESIAN_POINT ( 'NONE',  ( 16.88483580085999947, 8.492437095885001952, 7.591307468212999510 ) ) ;
#18740 = CARTESIAN_POINT ( 'NONE',  ( 21.34228936713000024, 9.218966921638999779, 0.000000000000000000 ) ) ;
#18741 = DIRECTION ( 'NONE',  ( 0.000000000000000000, 0.000000000000000000, -1.000000000000000000 ) ) ;
#18742 = CARTESIAN_POINT ( 'NONE',  ( 19.15656207941999867, 1.952743198197999908, 9.858894681773000102 ) ) ;
#18743 = CARTESIAN_POINT ( 'NONE',  ( 16.52299999999999969, -9.095294458157999529, 0.000000000000000000 ) ) ;
#18744 = ORIENTED_EDGE ( 'NONE', *, *, #7620, .F. ) ;
#18745 = CARTESIAN_POINT ( 'NONE',  ( 12.00945122375999929, 1.736409555422999906, -9.163372685490999814 ) ) ;
#18746 = DIRECTION ( 'NONE',  ( 0.000000000000000000, 0.000000000000000000, -1.000000000000000000 ) ) ;
#18747 = VECTOR ( 'NONE', #470, 1000.000000000000000 ) ;
#18748 = CARTESIAN_POINT ( 'NONE',  ( 4.518219764248003756, 12.29191853473001217, 1.948622234166999201 ) ) ;
#18749 = CARTESIAN_POINT ( 'NONE',  ( -0.3174390796334333187, 29.22271852741722853, -2.136439859271641595 ) ) ;
#18750 = CARTESIAN_POINT ( 'NONE',  ( -19.13615048806000019, -10.42776677607999858, -0.1439720813952999889 ) ) ;
#18751 = ORIENTED_EDGE ( 'NONE', *, *, #1103, .F. ) ;
#18752 = CARTESIAN_POINT ( 'NONE',  ( 0.5386878631261170502, 23.78722934400546762, 2.239973159359923915 ) ) ;
#18753 = ORIENTED_EDGE ( 'NONE', *, *, #22670, .F. ) ;
#18754 = CARTESIAN_POINT ( 'NONE',  ( 1.570067792648999871, 25.64723196749999801, 1.485270726656999996 ) ) ;
#18755 = CARTESIAN_POINT ( 'NONE',  ( 4.720426297672999816, 14.52234792950999243, 3.835364363128998644 ) ) ;
#18756 = CARTESIAN_POINT ( 'NONE',  ( 2.245636445399999737, 26.50799822781000259, -0.3106091461882000138 ) ) ;
#18757 = DIRECTION ( 'NONE',  ( 0.000000000000000000, 0.8660254037844288266, -0.5000000000000169864 ) ) ;
#18758 = DIRECTION ( 'NONE',  ( 1.000000000000000000, 0.000000000000000000, 0.000000000000000000 ) ) ;
#18759 = CARTESIAN_POINT ( 'NONE',  ( 12.45881424931000048, -1.641155845125999768, -10.50071198764000080 ) ) ;
#18760 = CARTESIAN_POINT ( 'NONE',  ( -13.60506528143999994, -10.72046298714999857, -0.8128029906560000351 ) ) ;
#18761 = CIRCLE ( 'NONE', #17623, 0.5000000000000004441 ) ;
#18762 = DIRECTION ( 'NONE',  ( 0.000000000000000000, 1.000000000000000000, 0.000000000000000000 ) ) ;
#18763 = CARTESIAN_POINT ( 'NONE',  ( -14.43045987140110498, 3.231330187236305385, 12.49999333232803700 ) ) ;
#18764 = ORIENTED_EDGE ( 'NONE', *, *, #8818, .T. ) ;
#18765 = SURFACE_SIDE_STYLE ('',( #2300 ) ) ;
#18766 = CARTESIAN_POINT ( 'NONE',  ( -0.5993264675742000502, 24.11013436640999785, -2.453430812916000292 ) ) ;
#18767 = CARTESIAN_POINT ( 'NONE',  ( 13.84793461847943696, -8.727815944628217082, 5.476926543191370733 ) ) ;
#18768 = CARTESIAN_POINT ( 'NONE',  ( -17.76455420454666978, 9.127155186021923328, -1.194614872368742198 ) ) ;
#18769 = CARTESIAN_POINT ( 'NONE',  ( 18.76610545325000245, 2.168194506458000159, 10.20310581668000083 ) ) ;
#18770 = CARTESIAN_POINT ( 'NONE',  ( -1.131706023269000161, 28.93810108242000112, -2.288580742153000003 ) ) ;
#18771 = CARTESIAN_POINT ( 'NONE',  ( 14.39816148159241749, -4.288529584651731064, 7.959032380803818363 ) ) ;
#18772 = CARTESIAN_POINT ( 'NONE',  ( 18.82462156322305447, -0.8953968736580824039, 10.44005362496722178 ) ) ;
#18773 = PLANE ( 'NONE',  #9881 ) ;
#18774 = DIRECTION ( 'NONE',  ( 0.000000000000000000, -1.000000000000000000, 0.000000000000000000 ) ) ;
#18775 = CONICAL_SURFACE ( 'NONE', #23027, 9.157130689899000586, 0.02565634000431304615 ) ;
#18776 = CARTESIAN_POINT ( 'NONE',  ( 24.28255857085423841, -12.88093503250115290, -2.689566074712900434 ) ) ;
#18777 = ORIENTED_EDGE ( 'NONE', *, *, #4655, .F. ) ;
#18778 = CARTESIAN_POINT ( 'NONE',  ( -14.09989322724901051, 9.032303263851988007, 3.309274488355915889E-05 ) ) ;
#18779 = CONICAL_SURFACE ( 'NONE', #20348, 4.309401076758999416, 1.119376321708719590 ) ;
#18780 = CARTESIAN_POINT ( 'NONE',  ( 2.100726171210397730, 23.93868288328740945, -1.266752783226519297 ) ) ;
#18781 = B_SPLINE_CURVE_WITH_KNOTS ( 'NONE', 3,
 ( #2480, #18711, #9869, #17254, #2122, #6231, #22339, #13612, #9392, #3946, #11341, #293, #7695, #15069, #12059, #19689, #779, #17503, #4913, #8179, #23053, #19190, #23184, #19569, #23299, #6714, #10235, #4674, #6600, #22935, #13860, #6352 ),
 .UNSPECIFIED., .F., .F.,
 ( 4, 2, 2, 2, 2, 2, 2, 2, 2, 2, 2, 2, 2, 2, 2, 4 ),
 ( 0.000000000000000000, 0.1249999999999996114, 0.1874999999999994171, 0.2187499999999992784, 0.2499999999999991118, 0.3124999999999990008, 0.3437499999999991118, 0.3749999999999992228, 0.4999999999999991118, 0.5624999999999991118, 0.5937499999999991118, 0.6249999999999991118, 0.6874999999999992228, 0.7187499999999992228, 0.7499999999999991118, 1.000000000000000000 ),
 .UNSPECIFIED. ) ;
#18782 = EDGE_LOOP ( 'NONE', ( #11359, #23682, #7767, #8766 ) ) ;
#18783 = DIRECTION ( 'NONE',  ( -8.659361257114346592E-17, 0.7071230553199298052, 0.7070905066786058457 ) ) ;
#18784 = DIRECTION ( 'NONE',  ( 1.000000000000000000, 0.000000000000000000, 0.000000000000000000 ) ) ;
#18785 = CARTESIAN_POINT ( 'NONE',  ( -23.75392841908999841, -7.466663059413999548, -11.77843647018000084 ) ) ;
#18786 = ORIENTED_EDGE ( 'NONE', *, *, #14420, .F. ) ;
#18787 = CARTESIAN_POINT ( 'NONE',  ( 16.97131495957000169, 6.714547727491000373, 8.817885161969000407 ) ) ;
#18788 = FACE_OUTER_BOUND ( 'NONE', #1000, .T. ) ;
#18789 = CARTESIAN_POINT ( 'NONE',  ( 2.387212940976999764, 27.84919433610000183, -1.595084814687000030 ) ) ;
#18790 = ORIENTED_EDGE ( 'NONE', *, *, #1343, .F. ) ;
#18791 = VERTEX_POINT ( 'NONE', #19894 ) ;
#18792 = CARTESIAN_POINT ( 'NONE',  ( -13.99999999999999467, 2.521425489992599189, -9.027018840861916971 ) ) ;
#18793 = CARTESIAN_POINT ( 'NONE',  ( 2.500000000000000000, 27.03419673618999752, 0.000000000000000000 ) ) ;
#18794 = PLANE ( 'NONE',  #11315 ) ;
#18795 = CARTESIAN_POINT ( 'NONE',  ( -14.44600786774907597, -9.403896164503946054, -8.711943152828570902 ) ) ;
#18796 = ADVANCED_FACE ( 'NONE', ( #14075 ), #19782, .T. ) ;
#18797 = ORIENTED_EDGE ( 'NONE', *, *, #11337, .T. ) ;
#18798 = CARTESIAN_POINT ( 'NONE',  ( 19.91708333333331993, -6.375401374836546786, 6.693310963685535242 ) ) ;
#18799 = CARTESIAN_POINT ( 'NONE',  ( 19.76435765169019021, 2.069040484427104420, -10.29933159267119791 ) ) ;
#18800 = AXIS2_PLACEMENT_3D ( 'NONE', #12311, #23310, #1641 ) ;
#18801 = CARTESIAN_POINT ( 'NONE',  ( 6.226186241163151003, 13.75890038697268025, 1.316088922015740570 ) ) ;
#18802 = CARTESIAN_POINT ( 'NONE',  ( 15.68554067004900787, -9.183687389534485490, 4.778903167209843872 ) ) ;
#18803 = B_SPLINE_CURVE_WITH_KNOTS ( 'NONE', 3,
 ( #23594, #18155, #5192, #16546, #12573, #23938, #7345, #14729, #4957, #5884, #11106, #5646, #11352, #11235, #2133, #22231, #14839, #13031, #3959, #7710, #18613, #16666, #13384, #425, #7577, #2018, #9407, #22353, #13270, #20430, #4191, #5771, #16776, #3839, #185, #20664, #20311, #14956, #18963, #13156, #2370, #9522, #72, #7947, #4074, #11468, #9292, #7825, #18723, #7457, #18844, #9759, #16899, #15196, #20784, #12913, #3716, #304, #18491, #2249, #15078, #9644, #17027, #22592, #17146, #1903, #542, #22474, #22124, #5998, #5533, #15441, #2615, #10006, #8436, #17268, #22707, #13874, #12190, #19077, #13744, #666, #19336, #21277, #19578, #21145, #6491, #10125, #8310, #13995, #17396, #11823, #790, #8190, #4558, #6241, #8072, #6117, #2863, #20908, #10373, #15558, #11950, #22827, #4313, #13624, #15674, #22946, #10247, #6362, #17763 ),
 .UNSPECIFIED., .F., .F.,
 ( 4, 2, 2, 2, 2, 2, 1, 2, 2, 2, 2, 2, 2, 2, 2, 2, 2, 2, 2, 2, 2, 2, 2, 2, 2, 2, 2, 2, 1, 2, 2, 2, 2, 2, 2, 2, 2, 2, 2, 2, 2, 2, 2, 2, 2, 2, 2, 2, 2, 2, 1, 2, 2, 2, 2, 2, 4 ),
 ( 0.000000000000000000, 0.01562500000000002776, 0.03125000000000005551, 0.04687500000000008327, 0.06250000000000011102, 0.07812500000000013878, 0.09375000000000016653, 0.1093750000000001943, 0.1250000000000002220, 0.1406250000000002498, 0.1562500000000002776, 0.1718750000000003053, 0.1875000000000003331, 0.2031250000000003608, 0.2187500000000003886, 0.2343750000000004163, 0.2500000000000003886, 0.2656250000000003886, 0.2812500000000004441, 0.2968750000000004441, 0.3125000000000004996, 0.3281250000000004996, 0.3437500000000005551, 0.3593750000000005551, 0.3750000000000006106, 0.4062500000000006106, 0.4375000000000006661, 0.4687500000000006661, 0.5000000000000006661, 0.5312500000000006661, 0.5625000000000007772, 0.5937500000000007772, 0.6250000000000008882, 0.6406250000000008882, 0.6562500000000008882, 0.6718750000000009992, 0.6875000000000009992, 0.7031250000000009992, 0.7187500000000009992, 0.7343750000000011102, 0.7500000000000011102, 0.7656250000000009992, 0.7812500000000008882, 0.7968750000000008882, 0.8125000000000007772, 0.8281250000000006661, 0.8437500000000005551, 0.8593750000000005551, 0.8750000000000004441, 0.8906250000000003331, 0.9062500000000002220, 0.9218750000000002220, 0.9375000000000001110, 0.9531250000000000000, 0.9687499999999998890, 0.9843750000000000000, 1.000000000000000000 ),
 .UNSPECIFIED. ) ;
#18804 = CARTESIAN_POINT ( 'NONE',  ( -14.61886126265999941, 9.861861598182999344, 4.891081622639000592 ) ) ;
#18805 = CARTESIAN_POINT ( 'NONE',  ( -0.9825804459669998936, 29.29200917197999843, -1.955293243215000087 ) ) ;
#18806 = CARTESIAN_POINT ( 'NONE',  ( -14.17369824411999879, 9.412195986946999327, 4.011894131497999005 ) ) ;
#18807 = ADVANCED_FACE ( 'NONE', ( #23520 ), #13731, .F. ) ;
#18808 = CARTESIAN_POINT ( 'NONE',  ( 1.414948191568242697, 29.69462877122279920, 1.631989406709256629 ) ) ;
#18809 = ORIENTED_EDGE ( 'NONE', *, *, #17869, .T. ) ;
#18810 = AXIS2_PLACEMENT_3D ( 'NONE', #2991, #15808, #2623 ) ;
#18811 = CARTESIAN_POINT ( 'NONE',  ( 1.908188185705999906, 24.96830048264000013, 1.057217360667000117 ) ) ;
#18812 = CARTESIAN_POINT ( 'NONE',  ( 19.24943393620590371, -8.016451796436484756, 6.770655802219995856 ) ) ;
#18813 = CARTESIAN_POINT ( 'NONE',  ( -19.23797835538982426, -7.594763024543788710, -7.229160888945107999 ) ) ;
#18814 = ORIENTED_EDGE ( 'NONE', *, *, #18719, .T. ) ;
#18815 = CARTESIAN_POINT ( 'NONE',  ( 23.99062354302999722, -6.216878364870000340, 12.50000000000000000 ) ) ;
#18816 = CARTESIAN_POINT ( 'NONE',  ( -5.155802126857005341, 15.83900978869999854, 2.700290858290999907 ) ) ;
#18817 = CARTESIAN_POINT ( 'NONE',  ( -13.99999999999999822, -9.953687737870106744, 2.637001505031396409 ) ) ;
#18818 = CARTESIAN_POINT ( 'NONE',  ( 14.35387625730999872, 4.075369344914999914, 8.193037116081999471 ) ) ;
#18819 = VERTEX_POINT ( 'NONE', #16251 ) ;
#18820 = B_SPLINE_CURVE_WITH_KNOTS ( 'NONE', 3,
 ( #735, #2812, #11889, #13451 ),
 .UNSPECIFIED., .F., .F.,
 ( 4, 4 ),
 ( 0.000000000000000000, 1.000000000000000000 ),
 .UNSPECIFIED. ) ;
#18821 = DIRECTION ( 'NONE',  ( 0.5000000000000169864, 0.000000000000000000, 0.8660254037844288266 ) ) ;
#18822 = CARTESIAN_POINT ( 'NONE',  ( 2.999999971291051892, 16.89999999999998437, -1.709463755659355061E-08 ) ) ;
#18823 = ADVANCED_FACE ( 'NONE', ( #19538 ), #23269, .F. ) ;
#18824 = VERTEX_POINT ( 'NONE', #5241 ) ;
#18825 = CARTESIAN_POINT ( 'NONE',  ( -16.66859587121331998, -7.950560622842369973, -4.582561865549370062 ) ) ;
#18826 = AXIS2_PLACEMENT_3D ( 'NONE', #5991, #15306, #13374 ) ;
#18827 = DIRECTION ( 'NONE',  ( -1.000000000000000000, 0.000000000000000000, 0.000000000000000000 ) ) ;
#18828 = CARTESIAN_POINT ( 'NONE',  ( -4.736842207410001393, 12.61338879614000241, -0.1498249729732001601 ) ) ;
#18829 = AXIS2_PLACEMENT_3D ( 'NONE', #16556, #12814, #20554 ) ;
#18830 = CARTESIAN_POINT ( 'NONE',  ( 12.00000000000000533, -4.155383997292160458, -8.661442538515151668 ) ) ;
#18831 = DIRECTION ( 'NONE',  ( 0.000000000000000000, -1.000000000000000000, 0.000000000000000000 ) ) ;
#18832 = CARTESIAN_POINT ( 'NONE',  ( -6.080190197657000084, 16.30605817606999608, -1.000000000000000000 ) ) ;
#18833 = CARTESIAN_POINT ( 'NONE',  ( 2.062331871376394954, 26.40495869946155594, -1.040606430369203750 ) ) ;
#18834 = AXIS2_PLACEMENT_3D ( 'NONE', #15622, #8378, #23131 ) ;
#18835 = CARTESIAN_POINT ( 'NONE',  ( 0.9358744650684699407, 26.41068681084919589, -4.078474779182607257 ) ) ;
#18836 = CARTESIAN_POINT ( 'NONE',  ( -0.3272492347489394104, 28.05086340285666324, -2.499999999999999112 ) ) ;
#18837 = ADVANCED_FACE ( 'NONE', ( #7051 ), #10254, .F. ) ;
#18838 = CARTESIAN_POINT ( 'NONE',  ( 0.8112170600937859133, 30.45292097617447524, 2.003657457152344890 ) ) ;
#18839 = ORIENTED_EDGE ( 'NONE', *, *, #14134, .F. ) ;
#18840 = CARTESIAN_POINT ( 'NONE',  ( -17.27916243917333361, 7.964251406370663311, 4.590452739718227093 ) ) ;
#18841 = CARTESIAN_POINT ( 'NONE',  ( 18.62845540657000143, -9.535387850010000221, -2.003629948511000070 ) ) ;
#18842 = CARTESIAN_POINT ( 'NONE',  ( 0.7581189486232848829, 12.82322678404221250, -6.625575084922103564 ) ) ;
#18843 = DIRECTION ( 'NONE',  ( 0.000000000000000000, 0.000000000000000000, -1.000000000000000000 ) ) ;
#18844 = CARTESIAN_POINT ( 'NONE',  ( -22.35796241690466601, 2.784267768755626982, -10.31842131618721936 ) ) ;
#18845 = CARTESIAN_POINT ( 'NONE',  ( 0.000000000000000000, -1.550000000000000044, 0.000000000000000000 ) ) ;
#18846 = VECTOR ( 'NONE', #9824, 1000.000000000000114 ) ;
#18847 = CARTESIAN_POINT ( 'NONE',  ( -6.000000000000000000, 26.50000000000000000, 1.229194263906000062 ) ) ;
#18848 = VERTEX_POINT ( 'NONE', #14433 ) ;
#18849 = EDGE_CURVE ( 'NONE', #9971, #11154, #12595, .T. ) ;
#18850 = FACE_OUTER_BOUND ( 'NONE', #19773, .T. ) ;
#18851 = CARTESIAN_POINT ( 'NONE',  ( -5.833999999999999631, 12.89775331292639926, 5.076162411588415241E-10 ) ) ;
#18852 = CIRCLE ( 'NONE', #21956, 14.43375672973999890 ) ;
#18853 = CARTESIAN_POINT ( 'NONE',  ( -1.009279597712957832, 28.56811160064914290, 1.920956085076729991 ) ) ;
#18854 = FACE_OUTER_BOUND ( 'NONE', #1100, .T. ) ;
#18855 = EDGE_CURVE ( 'NONE', #1169, #2559, #18207, .T. ) ;
#18856 = EDGE_CURVE ( 'NONE', #8479, #23530, #16047, .T. ) ;
#18857 = FACE_OUTER_BOUND ( 'NONE', #2846, .T. ) ;
#18858 = CARTESIAN_POINT ( 'NONE',  ( 15.20100174931000048, 0.8726850093137999975, 10.66462197497000020 ) ) ;
#18859 = CARTESIAN_POINT ( 'NONE',  ( -16.57879478578999866, 10.66533002439999933, 3.939376312692000504 ) ) ;
#18860 = CYLINDRICAL_SURFACE ( 'NONE', #12363, 3.000000000000000000 ) ;
#18861 = CARTESIAN_POINT ( 'NONE',  ( 13.83796080085999947, -10.41640823646999969, 4.395528184185000242 ) ) ;
#18862 = CARTESIAN_POINT ( 'NONE',  ( 1.065101660326078559, 24.49999999999999289, 2.250874270545449196 ) ) ;
#18863 = AXIS2_PLACEMENT_3D ( 'NONE', #17266, #4189, #11351 ) ;
#18864 = DIRECTION ( 'NONE',  ( 0.000000000000000000, 1.000000000000000000, 0.000000000000000000 ) ) ;
#18865 = CARTESIAN_POINT ( 'NONE',  ( 22.08360318395000021, -4.195824812958000471, -9.353156391488001375 ) ) ;
#18866 = EDGE_CURVE ( 'NONE', #23163, #8845, #22992, .T. ) ;
#18867 = CARTESIAN_POINT ( 'NONE',  ( 24.50000000000000000, -10.82531754731000007, 6.250000000000000000 ) ) ;
#18868 = ORIENTED_EDGE ( 'NONE', *, *, #9672, .F. ) ;
#18869 = CARTESIAN_POINT ( 'NONE',  ( 12.52254538689000007, 1.738956572546000112, -9.176809200813000444 ) ) ;
#18870 = CARTESIAN_POINT ( 'NONE',  ( -2.665093312283999705, 27.16206776952000013, 0.1571687770952999719 ) ) ;
#18871 = CARTESIAN_POINT ( 'NONE',  ( 4.793508155719999664, 12.39309388022998526, 1.113049502895999021 ) ) ;
#18872 = CARTESIAN_POINT ( 'NONE',  ( 2.500000000000000000, 30.23419673619000037, 0.000000000000000000 ) ) ;
#18873 = VECTOR ( 'NONE', #7159, 1000.000000000000000 ) ;
#18874 = CARTESIAN_POINT ( 'NONE',  ( -21.10023913963000197, -9.672014745719000217, -5.406718608085999911 ) ) ;
#18875 = VERTEX_POINT ( 'NONE', #5470 ) ;
#18876 = CARTESIAN_POINT ( 'NONE',  ( -19.35893705290999733, -9.828989445528000246, 3.502754984265999738 ) ) ;
#18877 = ORIENTED_EDGE ( 'NONE', *, *, #14522, .F. ) ;
#18878 = CARTESIAN_POINT ( 'NONE',  ( 0.4755391251864483082, 26.25858828695499270, 2.107219116345798948 ) ) ;
#18879 = CARTESIAN_POINT ( 'NONE',  ( -1.259486242684000112, 26.21549822780999861, 1.884954223019000175 ) ) ;
#18880 = DIRECTION ( 'NONE',  ( 0.000000000000000000, -0.9998336578527885488, -0.01823887673933978840 ) ) ;
#18881 = DIRECTION ( 'NONE',  ( 0.000000000000000000, 1.000000000000000000, 0.000000000000000000 ) ) ;
#18882 = CARTESIAN_POINT ( 'NONE',  ( 14.65256424931000190, 9.798150841947000700, -4.264230833847999946 ) ) ;
#18883 = EDGE_CURVE ( 'NONE', #7660, #17322, #16427, .T. ) ;
#18884 = EDGE_CURVE ( 'NONE', #4798, #10616, #16529, .T. ) ;
#18885 = CARTESIAN_POINT ( 'NONE',  ( -18.68332398068000089, -2.538655790982999871, -10.59268337770999935 ) ) ;
#18886 = DIRECTION ( 'NONE',  ( 0.000000000000000000, 0.000000000000000000, 1.000000000000000000 ) ) ;
#18887 = CARTESIAN_POINT ( 'NONE',  ( 24.18393254356861632, 13.26880198692879276, -2.017760803068382458 ) ) ;
#18888 = CIRCLE ( 'NONE', #11551, 4.000000000000000000 ) ;
#18889 = ORIENTED_EDGE ( 'NONE', *, *, #7459, .T. ) ;
#18890 = CARTESIAN_POINT ( 'NONE',  ( 2.521890885781000069, 24.68650439600999746, -0.1363133561440000030 ) ) ;
#18891 = VECTOR ( 'NONE', #21300, 1000.000000000000114 ) ;
#18892 = CARTESIAN_POINT ( 'NONE',  ( 14.33390021297796224, -4.407876064383785319, -9.345721391049526261 ) ) ;
#18893 = AXIS2_PLACEMENT_3D ( 'NONE', #7928, #17130, #10228 ) ;
#18894 = ORIENTED_EDGE ( 'NONE', *, *, #5556, .F. ) ;
#18895 = CARTESIAN_POINT ( 'NONE',  ( -0.8198258211412998708, 12.74638329176999996, -6.440467097934996055 ) ) ;
#18896 = CARTESIAN_POINT ( 'NONE',  ( -2.527261889986999854, 30.66151433680000338, -0.3618990238287000394 ) ) ;
#18897 = EDGE_CURVE ( 'NONE', #14252, #15392, #16957, .T. ) ;
#18898 = CARTESIAN_POINT ( 'NONE',  ( 11.66614181937426409, 3.921044720225134839, 12.49992990203553589 ) ) ;
#18899 = CARTESIAN_POINT ( 'NONE',  ( 18.85240113949000218, -1.886779804701000041, 10.26112574610000117 ) ) ;
#18900 = AXIS2_PLACEMENT_3D ( 'NONE', #23, #1731, #12863 ) ;
#18901 = CARTESIAN_POINT ( 'NONE',  ( -6.046835300290999804, 16.30334124114000360, 1.000000020649999932 ) ) ;
#18902 = CARTESIAN_POINT ( 'NONE',  ( 0.000000000000000000, 24.49999999999999645, -4.549999999999999822 ) ) ;
#18903 = EDGE_LOOP ( 'NONE', ( #23516, #13488, #21125, #3582, #3252, #10922 ) ) ;
#18904 = CARTESIAN_POINT ( 'NONE',  ( 1.350914310362234527, 29.97444252552742583, -3.838851412777819938 ) ) ;
#18905 = ORIENTED_EDGE ( 'NONE', *, *, #5622, .T. ) ;
#18906 = AXIS2_PLACEMENT_3D ( 'NONE', #2910, #17681, #21681 ) ;
#18907 = CARTESIAN_POINT ( 'NONE',  ( -2.016898400252999934, 25.75452502063999916, 1.850425600441000018 ) ) ;
#18908 = CARTESIAN_POINT ( 'NONE',  ( 24.35625626386759279, 9.206804001270699089, 9.053347694469197293 ) ) ;
#18909 = CARTESIAN_POINT ( 'NONE',  ( -0.6950034797113092688, 29.87418302490042876, -4.217541707417931107 ) ) ;
#18910 = EDGE_LOOP ( 'NONE', ( #16503, #144, #12983, #15798, #2298 ) ) ;
#18911 = VECTOR ( 'NONE', #22486, 1000.000000000000000 ) ;
#18912 = CARTESIAN_POINT ( 'NONE',  ( 17.69311855095000041, -10.67520284561000032, -3.052685539234999634 ) ) ;
#18913 = CARTESIAN_POINT ( 'NONE',  ( -1.500000000000000000, 7.100000000000000533, 0.000000000000000000 ) ) ;
#18914 = CARTESIAN_POINT ( 'NONE',  ( -2.804372049896000085, 25.80169433610000240, 0.6153010951427000386 ) ) ;
#18915 = ORIENTED_EDGE ( 'NONE', *, *, #12836, .T. ) ;
#18916 = VERTEX_POINT ( 'NONE', #9104 ) ;
#18917 = CARTESIAN_POINT ( 'NONE',  ( -24.49594166687720076, 10.56920153269230411, -6.693539566634715499 ) ) ;
#18918 = CARTESIAN_POINT ( 'NONE',  ( -10.70159721169000022, 15.56649841902000020, 0.2703010418137000714 ) ) ;
#18919 = CONICAL_SURFACE ( 'NONE', #5762, 1.949955127985000258, 0.7853751480324476786 ) ;
#18920 = CARTESIAN_POINT ( 'NONE',  ( 0.9039000843164147758, 6.837447795336954570, -1.500112088426254209 ) ) ;
#18921 = CARTESIAN_POINT ( 'NONE',  ( -24.43506354683044535, -9.928196662809744666, -7.803922592514855872 ) ) ;
#18922 = ORIENTED_EDGE ( 'NONE', *, *, #23322, .T. ) ;
#18923 = CARTESIAN_POINT ( 'NONE',  ( -23.44526871306000260, 9.800235893351999295, -2.981156924137000175 ) ) ;
#18924 = CARTESIAN_POINT ( 'NONE',  ( -14.50000018026810444, 10.69550487835361352, 6.474840093757361359 ) ) ;
#18925 = CARTESIAN_POINT ( 'NONE',  ( -23.74465998031000069, 6.216878364870000340, 12.50000000000000000 ) ) ;
#18926 = CARTESIAN_POINT ( 'NONE',  ( 15.32840305081342258, 1.511959382472310764, 10.25233748923334964 ) ) ;
#18927 = CARTESIAN_POINT ( 'NONE',  ( -13.77576579251999966, -10.20643469992999997, -2.518766116505000152 ) ) ;
#18928 = CIRCLE ( 'NONE', #13893, 6.125000000000000000 ) ;
#18929 = CARTESIAN_POINT ( 'NONE',  ( -0.7615468713905999554, 30.66386906700000026, -2.229746170830000374 ) ) ;
#18930 = AXIS2_PLACEMENT_3D ( 'NONE', #8577, #1426, #14261 ) ;
#18931 = VECTOR ( 'NONE', #560, 1000.000000000000000 ) ;
#18932 = CARTESIAN_POINT ( 'NONE',  ( -15.39248033193999987, -8.001506135565000122, 6.430926145009000727 ) ) ;
#18933 = CARTESIAN_POINT ( 'NONE',  ( 0.9667294541704517519, 29.66303702619708105, 1.931402186862774428 ) ) ;
#18934 = ORIENTED_EDGE ( 'NONE', *, *, #79, .T. ) ;
#18935 = CARTESIAN_POINT ( 'NONE',  ( 0.3893505392225000694, 24.16584150941000075, -2.150934381757999780 ) ) ;
#18936 = CARTESIAN_POINT ( 'NONE',  ( -17.87783718451543535, -7.209909598057388180, 7.565398080760625810 ) ) ;
#18937 = ORIENTED_EDGE ( 'NONE', *, *, #5842, .T. ) ;
#18938 = EDGE_CURVE ( 'NONE', #10250, #6636, #15124, .T. ) ;
#18939 = CARTESIAN_POINT ( 'NONE',  ( -5.079296814832000351, 15.76344662027999988, 2.859901774060001678 ) ) ;
#18940 = LINE ( 'NONE', #11442, #22306 ) ;
#18941 = CARTESIAN_POINT ( 'NONE',  ( 15.36750142131000096, -7.843339156370999099, -5.684071587432000250 ) ) ;
#18942 = EDGE_LOOP ( 'NONE', ( #16234, #17117, #23407 ) ) ;
#18943 = CARTESIAN_POINT ( 'NONE',  ( 18.48762270046333356, -8.239590629339057060, 4.107793420616442148 ) ) ;
#18944 = DIRECTION ( 'NONE',  ( 0.000000000000000000, -1.000000000000000000, 0.000000000000000000 ) ) ;
#18945 = ORIENTED_EDGE ( 'NONE', *, *, #2363, .T. ) ;
#18946 = CARTESIAN_POINT ( 'NONE',  ( 4.000000000000000000, 26.50000000000000355, 0.000000000000000000 ) ) ;
#18947 = DIRECTION ( 'NONE',  ( -0.4226182617406811226, 0.000000000000000000, 0.9063077870366585964 ) ) ;
#18948 = CARTESIAN_POINT ( 'NONE',  ( 4.722003391458004629, 12.53571431330998465, 0.2446935953583998513 ) ) ;
#18949 = DIRECTION ( 'NONE',  ( 1.000000000000000000, 0.000000000000000000, 2.391262342458999903E-11 ) ) ;
#18950 = VECTOR ( 'NONE', #11368, 999.9999999999998863 ) ;
#18951 = CARTESIAN_POINT ( 'NONE',  ( -21.49415997476000229, 2.491858532101999923, -9.269619466602000202 ) ) ;
#18952 = DIRECTION ( 'NONE',  ( -1.000000000000000000, -4.145989107584593997E-12, 0.000000000000000000 ) ) ;
#18953 = CARTESIAN_POINT ( 'NONE',  ( -12.25000000000000000, 1.374666032043000015E-14, 0.000000000000000000 ) ) ;
#18954 = CARTESIAN_POINT ( 'NONE',  ( -6.000000000000000000, 26.50000000000000000, 1.229194263906000062 ) ) ;
#18955 = CARTESIAN_POINT ( 'NONE',  ( 2.434931691670788823, 28.66753006952332683, -0.6543697108982007293 ) ) ;
#18956 = LINE ( 'NONE', #9753, #8401 ) ;
#18957 = CARTESIAN_POINT ( 'NONE',  ( 0.6841124492484266240, 30.44492334872505168, 2.049014591910544247 ) ) ;
#18958 = ORIENTED_EDGE ( 'NONE', *, *, #15031, .T. ) ;
#18959 = CARTESIAN_POINT ( 'NONE',  ( 21.91372127707999695, -5.477858186341999058, 8.167686895493000421 ) ) ;
#18960 = CARTESIAN_POINT ( 'NONE',  ( -2.791226855812472873, 13.06767197116077028, -6.129407314324748057 ) ) ;
#18961 = CARTESIAN_POINT ( 'NONE',  ( -23.62063575149434058, -8.943480941775941773, -2.984471859962635421 ) ) ;
#18962 = EDGE_CURVE ( 'NONE', #18824, #6273, #7393, .T. ) ;
#18963 = CARTESIAN_POINT ( 'NONE',  ( -22.94704266735730513, -10.35193671520849179, 2.143217020573386922 ) ) ;
#18964 = CARTESIAN_POINT ( 'NONE',  ( -2.451511826319000331, 27.60946440325999873, -0.2414528406811000116 ) ) ;
#18965 = DIRECTION ( 'NONE',  ( 1.000000000000000000, 0.000000000000000000, 0.000000000000000000 ) ) ;
#18966 = EDGE_LOOP ( 'NONE', ( #23920, #21516, #4103, #22781 ) ) ;
#18967 = CARTESIAN_POINT ( 'NONE',  ( -17.96347329169541496, 2.346826270286123339, 10.32639379259640400 ) ) ;
#18968 = CARTESIAN_POINT ( 'NONE',  ( 23.99062354302999722, 13.93375672974000068, -0.8660254037843999608 ) ) ;
#18969 = CARTESIAN_POINT ( 'NONE',  ( -1.269001982510553850, 28.30922767041318622, -1.762276763077230912 ) ) ;
#18970 = VERTEX_POINT ( 'NONE', #122 ) ;
#18971 = ADVANCED_FACE ( 'NONE', ( #11040 ), #18659, .T. ) ;
#18972 = ORIENTED_EDGE ( 'NONE', *, *, #6745, .F. ) ;
#18973 = CARTESIAN_POINT ( 'NONE',  ( -7.500000000000000000, 19.50000000000000000, -6.000000000000000000 ) ) ;
#18974 = CARTESIAN_POINT ( 'NONE',  ( 15.85912674931000055, -8.678267488395999152, -6.289192543930000490 ) ) ;
#18975 = DIRECTION ( 'NONE',  ( -0.000000000000000000, -1.000000000000000000, -0.000000000000000000 ) ) ;
#18976 = CARTESIAN_POINT ( 'NONE',  ( 12.95822370638999921, 3.216216234831999810, -9.637132962990998308 ) ) ;
#18977 = DIRECTION ( 'NONE',  ( 0.000000000000000000, -1.000000000000000000, 0.000000000000000000 ) ) ;
#18978 = DIRECTION ( 'NONE',  ( 0.000000000000000000, 1.000000000000000000, 0.000000000000000000 ) ) ;
#18979 = CARTESIAN_POINT ( 'NONE',  ( 21.82376044967999817, -7.488614721695999954, 6.188719846541999026 ) ) ;
#18980 = DIRECTION ( 'NONE',  ( 0.000000000000000000, -1.000000000000000000, 0.000000000000000000 ) ) ;
#18981 = ORIENTED_EDGE ( 'NONE', *, *, #15428, .T. ) ;
#18982 = DIRECTION ( 'NONE',  ( 1.000000000000000000, 0.000000000000000000, 0.000000000000000000 ) ) ;
#18983 = CARTESIAN_POINT ( 'NONE',  ( -2.329463490920999913, 28.81956776951999899, 1.304555153736000062 ) ) ;
#18984 = CARTESIAN_POINT ( 'NONE',  ( 2.263485475614001707, 11.78661699911999960, 4.163976765251001133 ) ) ;
#18985 = CARTESIAN_POINT ( 'NONE',  ( 2.114481634776250285, 29.03000053035885131, -0.4410627826741955748 ) ) ;
#18986 = ADVANCED_FACE ( 'NONE', ( #10 ), #18313, .F. ) ;
#18987 = CARTESIAN_POINT ( 'NONE',  ( -23.94067641790000067, 11.10629741394000014, 1.069876158558999979 ) ) ;
#18988 = VERTEX_POINT ( 'NONE', #14667 ) ;
#18989 = DIRECTION ( 'NONE',  ( 0.000000000000000000, 1.000000000000000000, 0.000000000000000000 ) ) ;
#18990 = VERTEX_POINT ( 'NONE', #20361 ) ;
#18991 = CARTESIAN_POINT ( 'NONE',  ( 0.000000000000000000, 15.00000000000000000, 0.000000000000000000 ) ) ;
#18992 = PLANE ( 'NONE',  #22835 ) ;
#18993 = CARTESIAN_POINT ( 'NONE',  ( -2.388357610153000188, 28.35256359723999964, -0.6232602838477999674 ) ) ;
#18994 = CARTESIAN_POINT ( 'NONE',  ( 0.9223941759128004847, 12.69701722427999790, 7.033009390352000345 ) ) ;
#18995 = CARTESIAN_POINT ( 'NONE',  ( 4.000000000000000000, 28.00000000000000000, 0.000000000000000000 ) ) ;
#18996 = CARTESIAN_POINT ( 'NONE',  ( 14.87193924930999955, 10.04572779547000039, 3.659788831486999960 ) ) ;
#18997 = EDGE_CURVE ( 'NONE', #19976, #9506, #14885, .T. ) ;
#18998 = CARTESIAN_POINT ( 'NONE',  ( -15.59561067990999916, -1.941903525450000112, 10.08593956198000008 ) ) ;
#18999 = CARTESIAN_POINT ( 'NONE',  ( 15.34106375730999972, -1.677480367812999917, -9.021981177529999840 ) ) ;
#19000 = DIRECTION ( 'NONE',  ( 0.000000000000000000, 0.000000000000000000, -1.000000000000000000 ) ) ;
#19001 = ORIENTED_EDGE ( 'NONE', *, *, #1722, .T. ) ;
#19002 = CARTESIAN_POINT ( 'NONE',  ( -1.650266299029000017, 30.34287082775999878, -2.167006502583999961 ) ) ;
#19003 = CARTESIAN_POINT ( 'NONE',  ( 1.465061595431000008, 24.55842216721000426, 2.057209151362000110 ) ) ;
#19004 = CARTESIAN_POINT ( 'NONE',  ( 4.691448533132819065, 14.73702420321861695, -3.942640714737680518 ) ) ;
#19005 = EDGE_LOOP ( 'NONE', ( #13552, #8913, #20375, #17191, #9598, #13324, #20818, #500 ) ) ;
#19006 = CYLINDRICAL_SURFACE ( 'NONE', #4853, 2.000000000000000000 ) ;
#19007 = DIRECTION ( 'NONE',  ( 0.000000000000000000, 0.5000000000000169864, -0.8660254037844288266 ) ) ;
#19008 = DIRECTION ( 'NONE',  ( 0.000000000000000000, 1.000000000000000000, 0.000000000000000000 ) ) ;
#19009 = CARTESIAN_POINT ( 'NONE',  ( 14.61207169101494685, -8.609499306320094192, 2.892750243897086904 ) ) ;
#19010 = CARTESIAN_POINT ( 'NONE',  ( 18.12769161559589293, 7.594118990230957600, -7.191324035859334884 ) ) ;
#19011 = DIRECTION ( 'NONE',  ( 0.000000000000000000, 0.000000000000000000, -1.000000000000000000 ) ) ;
#19012 =( NAMED_UNIT ( * ) PLANE_ANGLE_UNIT ( ) SI_UNIT ( $, .RADIAN. ) );
#19013 = EDGE_CURVE ( 'NONE', #5502, #9480, #16600, .T. ) ;
#19014 = CARTESIAN_POINT ( 'NONE',  ( 24.50000000000000000, -10.82531754731000007, -6.250000000000000000 ) ) ;
#19015 = EDGE_LOOP ( 'NONE', ( #20126, #10464, #1444, #8759 ) ) ;
#19016 = EDGE_CURVE ( 'NONE', #6411, #3590, #2065, .T. ) ;
#19017 = LINE ( 'NONE', #3899, #9226 ) ;
#19018 = VERTEX_POINT ( 'NONE', #234 ) ;
#19019 = DIRECTION ( 'NONE',  ( 0.000000000000000000, 0.000000000000000000, -1.000000000000000000 ) ) ;
#19020 = CIRCLE ( 'NONE', #1247, 1.999999999999998668 ) ;
#19022 = CARTESIAN_POINT ( 'NONE',  ( 1.713341213838733612, 24.28993051964441463, -1.368779845717938315 ) ) ;
#19021 = CARTESIAN_POINT ( 'NONE',  ( -3.079591938543706497, 11.88219301979877862, 3.716998605068117634 ) ) ;
#19023 = CARTESIAN_POINT ( 'NONE',  ( -1.099193499486128323, 29.93562577624026488, -3.984182490697167900 ) ) ;
#19024 = CARTESIAN_POINT ( 'NONE',  ( 6.175768678244707210, 13.98844511635596177, -0.6082058386448220277 ) ) ;
#19025 = CARTESIAN_POINT ( 'NONE',  ( -7.128598361965003960, 15.40011789705998702, -1.088345829342000526 ) ) ;
#19026 = CARTESIAN_POINT ( 'NONE',  ( 0.000000000000000000, 14.95000002005000006, -4.674999979945999584 ) ) ;
#19027 = EDGE_CURVE ( 'NONE', #20904, #10478, #3320, .T. ) ;
#19028 = ORIENTED_EDGE ( 'NONE', *, *, #11737, .F. ) ;
#19029 = ORIENTED_EDGE ( 'NONE', *, *, #5216, .T. ) ;
#19030 = EDGE_CURVE ( 'NONE', #2430, #19423, #4248, .T. ) ;
#19031 = CARTESIAN_POINT ( 'NONE',  ( 5.699442596042000098, 1.578914512950999657E-14, -14.15464499511999996 ) ) ;
#19032 = CARTESIAN_POINT ( 'NONE',  ( -1.708192668324312713, 6.989350524238209239, -0.4397697262170950916 ) ) ;
#19033 = CARTESIAN_POINT ( 'NONE',  ( -24.48376588670980070, -10.31426502621016006, -7.135315508364757697 ) ) ;
#19034 = ORIENTED_EDGE ( 'NONE', *, *, #8801, .T. ) ;
#19035 = CARTESIAN_POINT ( 'NONE',  ( -22.41706829942000212, -10.13657052992000196, -1.268620720673999891 ) ) ;
#19036 = CARTESIAN_POINT ( 'NONE',  ( -14.45960647534970889, 9.597314625695767987, 8.376896358970226331 ) ) ;
#19037 = CARTESIAN_POINT ( 'NONE',  ( 6.226910483035863919, 13.75536151932502449, 1.330040350533948423 ) ) ;
#19038 = CARTESIAN_POINT ( 'NONE',  ( 15.58002254845384016, -6.890210661546990245, 7.720466256389740600 ) ) ;
#19039 = B_SPLINE_CURVE_WITH_KNOTS ( 'NONE', 3,
 ( #18867, #2272, #9665, #14262, #6746, #8329, #19726, #14019, #10150, #12455, #6630, #6383 ),
 .UNSPECIFIED., .F., .F.,
 ( 4, 1, 1, 1, 1, 2, 2, 4 ),
 ( 0.000000000000000000, 0.2499999999999986122, 0.3749999999999980571, 0.4374999999999979461, 0.4687499999999978351, 0.4843749999999980016, 0.4999999999999981126, 1.000000000000000000 ),
 .UNSPECIFIED. ) ;
#19040 = CARTESIAN_POINT ( 'NONE',  ( -19.79001396229000065, -7.801656982797999795, 6.945750858680000306 ) ) ;
#19041 = CARTESIAN_POINT ( 'NONE',  ( -1.837043917312000119, 30.73580608766999944, -1.475520569229000101 ) ) ;
#19042 = CARTESIAN_POINT ( 'NONE',  ( -18.63376253787999914, -9.149460784975000038, 0.000000000000000000 ) ) ;
#19043 = AXIS2_PLACEMENT_3D ( 'NONE', #17590, #984, #15873 ) ;
#19044 = CARTESIAN_POINT ( 'NONE',  ( -12.95491615630000126, -0.8957832334074999903, -10.15856198502000041 ) ) ;
#19045 = CARTESIAN_POINT ( 'NONE',  ( 0.3079095288441306422, 29.62188598588733868, 2.138016069174891953 ) ) ;
#19046 = VERTEX_POINT ( 'NONE', #10059 ) ;
#19047 = CARTESIAN_POINT ( 'NONE',  ( 1.079791510068999871, 24.65442586790999968, 1.900569086254999984 ) ) ;
#19048 = CARTESIAN_POINT ( 'NONE',  ( -19.15116083384464574, -5.105618582937671235, -9.150693563290923649 ) ) ;
#19049 = ORIENTED_EDGE ( 'NONE', *, *, #11754, .F. ) ;
#19050 = CARTESIAN_POINT ( 'NONE',  ( -2.246347731941017223, 24.65365226805931087, -5.222125272214524731E-08 ) ) ;
#19051 = CARTESIAN_POINT ( 'NONE',  ( -2.399999999999999911, 28.00000000000000000, 0.000000000000000000 ) ) ;
#19052 = CARTESIAN_POINT ( 'NONE',  ( -2.147180172777956919, 30.84444203262654938, 0.1925145778103813932 ) ) ;
#19053 = CARTESIAN_POINT ( 'NONE',  ( -20.29659587121332365, -8.031911560230602376, -4.629449613728698232 ) ) ;
#19054 = CARTESIAN_POINT ( 'NONE',  ( 14.70937642131000089, 0.7886220128679000130, 9.636901145054999063 ) ) ;
#19055 = ORIENTED_EDGE ( 'NONE', *, *, #14723, .T. ) ;
#19056 = CARTESIAN_POINT ( 'NONE',  ( -6.232893174142998483, 15.85796039161002824, -1.061654000538000409 ) ) ;
#19057 = FACE_OUTER_BOUND ( 'NONE', #132, .T. ) ;
#19058 = B_SPLINE_SURFACE_WITH_KNOTS ( 'NONE', 3, 3, ( 
 ( #12653, #16274, #16024, #8785, #7187, #21742, #5156, #23780, #10720, #12537, #3568, #19924, #18338, #3342, #1518, #23666, #21856, #5267, #15906, #13232, #264, #7670, #22553, #5496, #5959, #9252, #13344, #12876, #20744, #16629, #20395, #3801, #2212, #11071, #16509 ),
 ( #3921, #11313, #18689, #20276, #14695, #15043, #4151, #7541, #22439, #2095, #9485, #7788, #11194, #14804, #23898, #39, #20625, #7421, #18454, #7305, #4035, #22087, #11548, #149, #3680, #16862, #5849, #11429, #18804, #9604, #16990, #391, #13118, #18927, #15158 ),
 ( #1864, #9134, #1982, #5732, #22199, #5612, #12994, #18577, #9365, #22315, #16739, #14921, #20516, #15759, #6443, #6322, #12149, #992, #11784, #4642, #12030, #17347, #10086, #13467, #20983, #4394, #2825, #19412, #13954, #19159, #17473, #4279, #15518, #623, #15635 ),
 ( #19040, #21230, #6202, #867, #15275, #9842, #22906, #15397, #13707, #2449, #8024, #22786, #749, #11905, #13587, #21348, #10205, #17599, #8153, #8394, #8271, #23150, #22667, #21100, #20869, #23026, #19289, #13831, #2570, #4515, #9960, #6570, #2702, #4763, #2337 ) ),
 .UNSPECIFIED., .F., .F., .F.,
 ( 4, 4 ),
 ( 4, 1, 1, 1, 1, 1, 1, 1, 1, 1, 1, 1, 1, 1, 1, 1, 1, 1, 1, 1, 1, 1, 1, 1, 1, 1, 1, 1, 1, 1, 1, 1, 4 ),
 ( -0.6000240009601000013, 1.600024000959999970 ),
 ( -0.01778791961293000115, 0.01111744975807999955, 0.04002281912908000477, 0.06892818850008999854, 0.09783355787108999335, 0.1267389272420999802, 0.1556442966131000027, 0.1845496659840999976, 0.2134550353551000201, 0.2423604047261000149, 0.2712657740971000098, 0.3001711434680999768, 0.3290765128390999994, 0.3579818822100999665, 0.3868872515810999890, 0.4157926209521000116, 0.4446979903232000098, 0.4736033596941999768, 0.5025087290651999439, 0.5314140984361999109, 0.5603194678071999890, 0.5892248371781999561, 0.6181302065492000342, 0.6470355759202000012, 0.6759409452911999683, 0.7048463146621999353, 0.7337516840332000134, 0.7626570534041999805, 0.7915624227752000586, 0.8204677921462000256, 0.8493731615171999927, 0.8782785308881999597, 0.9071839002592000378 ),
 .UNSPECIFIED. ) ;
#19059 = ORIENTED_EDGE ( 'NONE', *, *, #3604, .T. ) ;
#19060 = CARTESIAN_POINT ( 'NONE',  ( -2.008209816024387084, 24.68901357082605585, 0.9452844701119602622 ) ) ;
#19061 = FACE_OUTER_BOUND ( 'NONE', #21593, .T. ) ;
#19062 = CARTESIAN_POINT ( 'NONE',  ( -3.187683228664999646, 12.10419657022999651, 3.627759556269996910 ) ) ;
#19063 = CARTESIAN_POINT ( 'NONE',  ( -14.00000000000000000, -2.869707268214888529, 9.513533945855728646 ) ) ;
#19064 = CARTESIAN_POINT ( 'NONE',  ( 17.71169237777402827, -10.07440819872460658, -2.697916929237545780 ) ) ;
#19065 = CARTESIAN_POINT ( 'NONE',  ( 18.75008227645999881, 0.000000000000000000, 0.000000000000000000 ) ) ;
#19066 = CARTESIAN_POINT ( 'NONE',  ( 18.77245603379665795, -7.997832810931552849, -4.609517281848381387 ) ) ;
#19067 = CARTESIAN_POINT ( 'NONE',  ( -6.147399691167000135, 16.31019195569000146, -0.9999999999994999555 ) ) ;
#19068 = CARTESIAN_POINT ( 'NONE',  ( -1.678813317411953498, 26.50000000000001066, 3.649538832790644616 ) ) ;
#19069 = CARTESIAN_POINT ( 'NONE',  ( -2.184465970885646424, 28.16753006952332683, -1.259047450927245126 ) ) ;
#19070 = CARTESIAN_POINT ( 'NONE',  ( 2.158678543002582106, 30.61128633804222687, -0.1265477462312649959 ) ) ;
#19071 = ORIENTED_EDGE ( 'NONE', *, *, #4700, .T. ) ;
#19072 = DIRECTION ( 'NONE',  ( 0.5000000000000172085, -0.8660254037844288266, 0.000000000000000000 ) ) ;
#19073 = B_SPLINE_CURVE_WITH_KNOTS ( 'NONE', 3,
 ( #11304, #4143, #17100, #7781, #257, #1974, #20736, #9358, #11540, #18920, #22191, #16731, #2327, #7662, #497, #7899, #15267, #22659, #12869, #3673, #23020, #22899, #6563, #11659, #6068, #6196, #15752, #4635, #23140, #19032, #6436, #19280 ),
 .UNSPECIFIED., .F., .F.,
 ( 4, 2, 2, 2, 2, 2, 2, 2, 2, 2, 2, 2, 2, 2, 2, 4 ),
 ( 0.000000000000000000, 0.06249999999999993061, 0.1249999999999998612, 0.2499999999999998335, 0.3124999999999998890, 0.3437499999999998890, 0.3749999999999998890, 0.4374999999999998335, 0.4999999999999997780, 0.5624999999999996669, 0.5937499999999996669, 0.6093749999999996669, 0.6249999999999996669, 0.7499999999999997780, 0.8749999999999998890, 1.000000000000000000 ),
 .UNSPECIFIED. ) ;
#19074 = CARTESIAN_POINT ( 'NONE',  ( 4.321647192813569127, 13.42637534801005117, -5.297716879388643108 ) ) ;
#19075 = PRODUCT_DEFINITION_FORMATION_WITH_SPECIFIED_SOURCE ( 'ANY', '', #15579, .NOT_KNOWN. ) ;
#19076 = CARTESIAN_POINT ( 'NONE',  ( 2.500000000000000000, 27.83419673618999823, 0.000000000000000000 ) ) ;
#19077 = CARTESIAN_POINT ( 'NONE',  ( -20.61749804056798752, 0.1139427650053814606, -10.51009152996787144 ) ) ;
#19078 = CARTESIAN_POINT ( 'NONE',  ( 1.203722632180999952, 25.75696440325999959, -2.149413090608000232 ) ) ;
#19079 = CARTESIAN_POINT ( 'NONE',  ( 12.50898179946000077, -7.466908609752000103, 11.77829470162000014 ) ) ;
#19080 = ORIENTED_EDGE ( 'NONE', *, *, #17636, .F. ) ;
#19081 = CARTESIAN_POINT ( 'NONE',  ( -18.71707669688263920, 3.197755709358065523, -9.964328844018272235 ) ) ;
#19082 = CARTESIAN_POINT ( 'NONE',  ( -2.500000000000000000, 27.43419673618999965, 0.000000000000000000 ) ) ;
#19083 = DIRECTION ( 'NONE',  ( 0.000000000000000000, 0.000000000000000000, -1.000000000000000000 ) ) ;
#19084 = CYLINDRICAL_SURFACE ( 'NONE', #13825, 4.750000000000000000 ) ;
#19085 = ORIENTED_EDGE ( 'NONE', *, *, #3353, .T. ) ;
#19086 = CARTESIAN_POINT ( 'NONE',  ( 4.000000000000000888, 29.89685207198628092, -1.322601766568780146 ) ) ;
#19087 = B_SPLINE_CURVE_WITH_KNOTS ( 'NONE', 3,
 ( #4565, #13751, #23068, #7953 ),
 .UNSPECIFIED., .F., .F.,
 ( 4, 4 ),
 ( 0.000000000000000000, 1.000000000000000000 ),
 .UNSPECIFIED. ) ;
#19088 = CARTESIAN_POINT ( 'NONE',  ( 17.94318924931000225, -0.08898103000111000360, -10.77198407497000154 ) ) ;
#19089 = CIRCLE ( 'NONE', #2088, 2.500000000000000000 ) ;
#19090 = CARTESIAN_POINT ( 'NONE',  ( -24.32811878836000119, 9.771184119221999254, -4.393942764655000666 ) ) ;
#19091 = ADVANCED_FACE ( 'NONE', ( #15364 ), #19006, .T. ) ;
#19092 = CARTESIAN_POINT ( 'NONE',  ( -19.08240939882999854, 4.922202718798000198, -9.729665371451000411 ) ) ;
#19093 = PLANE ( 'NONE',  #715 ) ;
#19094 = CARTESIAN_POINT ( 'NONE',  ( 18.78114037306000128, 10.87330394281000068, 0.8145811978064999570 ) ) ;
#19095 = DIRECTION ( 'NONE',  ( 0.8206518289197470839, 0.5714285394436248167, 4.207942230546201995E-10 ) ) ;
#19096 = CARTESIAN_POINT ( 'NONE',  ( 0.000000000000000000, 21.94999982584599962, 0.000000000000000000 ) ) ;
#19097 = CARTESIAN_POINT ( 'NONE',  ( 21.64671134753000104, -2.561010203381999695, 9.366262177596999194 ) ) ;
#19098 = CARTESIAN_POINT ( 'NONE',  ( 4.000024251878889991, 24.52555747447230416, -0.7498250608958109131 ) ) ;
#19099 = ORIENTED_EDGE ( 'NONE', *, *, #17334, .F. ) ;
#19100 = CIRCLE ( 'NONE', #2473, 2.999999999999999112 ) ;
#19101 = CARTESIAN_POINT ( 'NONE',  ( -6.042815635770000249, 16.39253429789999927, 0.9999999720525000191 ) ) ;
#19102 = CARTESIAN_POINT ( 'NONE',  ( -2.388357610153000188, 28.61663313895000016, -0.6232602838477999674 ) ) ;
#19103 = CARTESIAN_POINT ( 'NONE',  ( 4.336915520410000724, 12.38777958348998709, 1.884790593294000782 ) ) ;
#19104 = CARTESIAN_POINT ( 'NONE',  ( 2.124360424174371431, 29.02695534453464532, -0.3899590626965727114 ) ) ;
#19105 = EDGE_CURVE ( 'NONE', #21343, #15280, #21069, .T. ) ;
#19106 = CARTESIAN_POINT ( 'NONE',  ( -22.12320936320999820, 10.23231788766999983, -4.323895602960999618 ) ) ;
#19107 = ORIENTED_EDGE ( 'NONE', *, *, #18548, .T. ) ;
#19108 = DIRECTION ( 'NONE',  ( -0.8193292504149961575, 0.000000000000000000, -0.5733232765328829528 ) ) ;
#19109 = ORIENTED_EDGE ( 'NONE', *, *, #9534, .T. ) ;
#19110 = CARTESIAN_POINT ( 'NONE',  ( -24.24003052286102999, 3.589673254490056031, -12.49985157729351215 ) ) ;
#19111 = CARTESIAN_POINT ( 'NONE',  ( -4.749994070560452641, 12.54999978084880752, 0.6289937086464317817 ) ) ;
#19112 = CARTESIAN_POINT ( 'NONE',  ( 4.878286811419003222, 14.94151125082000497, 3.715753592770002722 ) ) ;
#19113 = DIRECTION ( 'NONE',  ( 0.000000000000000000, 1.000000000000000000, 0.000000000000000000 ) ) ;
#19114 = CARTESIAN_POINT ( 'NONE',  ( 12.67818924931000168, 6.046592098211998945, -8.747551238178997934 ) ) ;
#19115 = CARTESIAN_POINT ( 'NONE',  ( -16.65202050098999820, 5.360250747359000201, -9.417511137717001546 ) ) ;
#19116 = CARTESIAN_POINT ( 'NONE',  ( 13.80543875730999837, 6.427790461817999734, -6.492639392963999612 ) ) ;
#19117 = CARTESIAN_POINT ( 'NONE',  ( 18.94203808734637207, 2.038145998098363609, 10.23480975536132220 ) ) ;
#19118 = ADVANCED_FACE ( 'NONE', ( #6044 ), #12907, .F. ) ;
#19119 = VERTEX_POINT ( 'NONE', #13674 ) ;
#19120 = CARTESIAN_POINT ( 'NONE',  ( 13.50000000000000000, -4.002954420673999536, -8.080569262580000967 ) ) ;
#19121 = CARTESIAN_POINT ( 'NONE',  ( 2.306244679868000080, 25.51903888322000213, -0.7375453083353000761 ) ) ;
#19122 = CARTESIAN_POINT ( 'NONE',  ( 14.00976417969420851, -10.32366805564640799, -0.007670053520953104033 ) ) ;
#19123 = AXIS2_PLACEMENT_3D ( 'NONE', #16231, #1221, #1468 ) ;
#19124 = ORIENTED_EDGE ( 'NONE', *, *, #17713, .F. ) ;
#19125 = CARTESIAN_POINT ( 'NONE',  ( 1.712095296464997585, 13.93444603479998811, -5.928653740531998118 ) ) ;
#19126 = CARTESIAN_POINT ( 'NONE',  ( -24.11803009774155626, 13.00903097541294073, -2.467105211237874851 ) ) ;
#19127 = CARTESIAN_POINT ( 'NONE',  ( -2.408156795220000479, 29.83799085022999975, 1.318887963389000051 ) ) ;
#19128 = CARTESIAN_POINT ( 'NONE',  ( 11.31235608929811498, -2.505169353225074058, 12.49996790083181963 ) ) ;
#19129 = CARTESIAN_POINT ( 'NONE',  ( 17.40288447006501826, -10.49761850512724415, 1.364539225918563359 ) ) ;
#19130 = CARTESIAN_POINT ( 'NONE',  ( -14.25699038479000080, -13.93375672974000068, 0.000000000000000000 ) ) ;
#19131 = VECTOR ( 'NONE', #20489, 1000.000000000000000 ) ;
#19132 = CARTESIAN_POINT ( 'NONE',  ( -6.250000000000000000, 1.301187224093999891E-14, 0.000000000000000000 ) ) ;
#19133 = EDGE_CURVE ( 'NONE', #23444, #14865, #17817, .T. ) ;
#19134 = DIRECTION ( 'NONE',  ( 0.000000000000000000, 1.000000000000000000, 0.000000000000000000 ) ) ;
#19135 = VERTEX_POINT ( 'NONE', #19630 ) ;
#19136 = CARTESIAN_POINT ( 'NONE',  ( 0.6252065045458350401, 11.57481763370839545, -4.750366986350042176 ) ) ;
#19137 = ORIENTED_EDGE ( 'NONE', *, *, #11710, .T. ) ;
#19138 = CARTESIAN_POINT ( 'NONE',  ( -4.750000000000000000, 22.19999999999999574, 0.000000000000000000 ) ) ;
#19140 = CARTESIAN_POINT ( 'NONE',  ( 2.147292731478545935, 24.17747261322704233, 0.4479935266175709141 ) ) ;
#19139 = CARTESIAN_POINT ( 'NONE',  ( -1.987853604051396106, 11.65079879119223349, 4.388780662035608238 ) ) ;
#19141 = CARTESIAN_POINT ( 'NONE',  ( -1.989999999999999991, 9.000000000000000000, -7.500000000000000000 ) ) ;
#19142 = CONICAL_SURFACE ( 'NONE', #11032, 4.309401076758999416, 1.119376321708719590 ) ;
#19143 = CARTESIAN_POINT ( 'NONE',  ( 15.49387847584000077, -0.07844713208112001623, 11.04258953166000090 ) ) ;
#19144 = PLANE ( 'NONE',  #12906 ) ;
#19145 = ADVANCED_FACE ( 'NONE', ( #1580 ), #1086, .F. ) ;
#19146 = DIRECTION ( 'NONE',  ( 0.000000000000000000, -1.000000000000000000, 0.000000000000000000 ) ) ;
#19147 = EDGE_LOOP ( 'NONE', ( #7105, #22532, #640, #15258, #7783, #11201 ) ) ;
#19148 = EDGE_LOOP ( 'NONE', ( #15107, #13094, #20152, #23916, #13634, #19714 ) ) ;
#19149 = CARTESIAN_POINT ( 'NONE',  ( -14.00000000000000178, -6.309619694642019994, -7.620818005153923380 ) ) ;
#19150 = DIRECTION ( 'NONE',  ( -1.000000000000000000, 0.000000000000000000, 0.000000000000000000 ) ) ;
#19151 = FACE_BOUND ( 'NONE', #6951, .T. ) ;
#19152 = EDGE_CURVE ( 'NONE', #2047, #6636, #19547, .T. ) ;
#19153 = ORIENTED_EDGE ( 'NONE', *, *, #8754, .F. ) ;
#19154 = CARTESIAN_POINT ( 'NONE',  ( -19.43131210050000135, 9.425945272632999306, 1.879262601378000053 ) ) ;
#19155 = EDGE_CURVE ( 'NONE', #19300, #15250, #21479, .T. ) ;
#19156 = CARTESIAN_POINT ( 'NONE',  ( 1.700000000000000622, 12.91217734593225863, -1.053565373075000977 ) ) ;
#19157 = CARTESIAN_POINT ( 'NONE',  ( 6.185782116123350605, 13.94105495766904390, 0.7320468670209526740 ) ) ;
#19158 = CARTESIAN_POINT ( 'NONE',  ( 15.88509334382326443, -10.12552540729580564, -2.174043714885656620 ) ) ;
#19159 = CARTESIAN_POINT ( 'NONE',  ( -14.58481954452000018, 5.127933381152999459, 9.739763264848999569 ) ) ;
#19160 = FACE_OUTER_BOUND ( 'NONE', #18215, .T. ) ;
#19161 = CARTESIAN_POINT ( 'NONE',  ( -20.74166715155477192, 2.803544456025320208, -10.13304684785263454 ) ) ;
#19162 = CONICAL_SURFACE ( 'NONE', #12974, 4.674999979945999584, 0.7853981633972997312 ) ;
#19163 = CARTESIAN_POINT ( 'NONE',  ( -23.80485347273356211, -1.053090434097245121, -9.586785637656749515 ) ) ;
#19164 = CARTESIAN_POINT ( 'NONE',  ( -2.122079233582688573, 29.37598636205398961, -0.4706325729297383687 ) ) ;
#19165 = EDGE_CURVE ( 'NONE', #21798, #1224, #18374, .T. ) ;
#19166 = ORIENTED_EDGE ( 'NONE', *, *, #14550, .F. ) ;
#19167 = B_SPLINE_CURVE_WITH_KNOTS ( 'NONE', 3,
 ( #17157, #15686, #552, #17409, #19086, #1046, #802, #8203, #15206, #22957 ),
 .UNSPECIFIED., .F., .F.,
 ( 4, 1, 1, 2, 2, 4 ),
 ( 0.000000000000000000, 0.2500000000000013323, 0.3750000000000016098, 0.4375000000000018874, 0.5000000000000021094, 1.000000000000000000 ),
 .UNSPECIFIED. ) ;
#19168 = CARTESIAN_POINT ( 'NONE',  ( -0.1537472993604999949, 23.39806608891999673, -2.073430105596999695 ) ) ;
#19169 = EDGE_CURVE ( 'NONE', #17309, #2115, #12197, .T. ) ;
#19170 = CARTESIAN_POINT ( 'NONE',  ( -15.44694658125069608, -2.463998168450752146, -10.08867902004827677 ) ) ;
#19171 =( REPRESENTATION_RELATIONSHIP ('NONE','NONE', #13682, #12781 ) REPRESENTATION_RELATIONSHIP_WITH_TRANSFORMATION ( #5174 )SHAPE_REPRESENTATION_RELATIONSHIP( ) );
#19172 = ORIENTED_EDGE ( 'NONE', *, *, #4520, .F. ) ;
#19173 = CARTESIAN_POINT ( 'NONE',  ( -2.151153546426574525, 24.62672406677130255, -0.7503138593518134947 ) ) ;
#19174 = CARTESIAN_POINT ( 'NONE',  ( 4.817436639547997501, 14.48250318153000471, -3.715459049975000205 ) ) ;
#19175 = CARTESIAN_POINT ( 'NONE',  ( -2.125241982083288850, 30.86478522159566751, 0.2061377204366061922 ) ) ;
#19176 = CARTESIAN_POINT ( 'NONE',  ( -19.57855420454666984, 9.173706001228294937, -1.200708359830031657 ) ) ;
#19177 = CARTESIAN_POINT ( 'NONE',  ( 13.61250142131000196, -6.495520710102000272, -7.123429297049000297 ) ) ;
#19178 = EDGE_LOOP ( 'NONE', ( #21727, #313, #7416 ) ) ;
#19179 = VECTOR ( 'NONE', #18517, 1000.000000000000000 ) ;
#19180 = CARTESIAN_POINT ( 'NONE',  ( 18.35395603379666341, -5.527903405087061905, 7.358200411944897823 ) ) ;
#19181 = CARTESIAN_POINT ( 'NONE',  ( 0.000000000000000000, 24.80000000000000426, -4.618802153517000519 ) ) ;
#19182 = LINE ( 'NONE', #15062, #9425 ) ;
#19183 = ORIENTED_EDGE ( 'NONE', *, *, #3498, .T. ) ;
#19184 = CARTESIAN_POINT ( 'NONE',  ( 24.24531177150999994, 0.000000000000000000, 0.000000000000000000 ) ) ;
#19185 = DIRECTION ( 'NONE',  ( -0.9999999999999998890, -9.268909281637997623E-09, 3.975906136097999155E-09 ) ) ;
#19186 = CARTESIAN_POINT ( 'NONE',  ( 23.85298513858829139, 10.35157075127159487, 2.356844212935751859 ) ) ;
#19187 = LINE ( 'NONE', #22931, #9499 ) ;
#19188 = CARTESIAN_POINT ( 'NONE',  ( 18.10698583361175551, 0.6240570753724111741, -10.40424229370149689 ) ) ;
#19189 = CARTESIAN_POINT ( 'NONE',  ( 4.834782059083999606, 12.44497316928999808, -0.3759403457470999466 ) ) ;
#19190 = CARTESIAN_POINT ( 'NONE',  ( -14.48875658296588398, 11.47331197282439774, -5.127631166282751174 ) ) ;
#19191 = CARTESIAN_POINT ( 'NONE',  ( 22.29042311570000123, 0.6833233609315999546, 11.23355659561000053 ) ) ;
#19192 = CARTESIAN_POINT ( 'NONE',  ( -12.25000000000000000, 13.93375672974000068, 0.000000000000000000 ) ) ;
#19193 = CARTESIAN_POINT ( 'NONE',  ( -3.644450799678000230, 14.33206891749000000, -4.922778709793999674 ) ) ;
#19194 = DIRECTION ( 'NONE',  ( 0.000000000000000000, 1.000000000000000000, 0.000000000000000000 ) ) ;
#19195 = CARTESIAN_POINT ( 'NONE',  ( -2.106357140788216675, 30.17536992306000343, -0.4799468061218781223 ) ) ;
#19196 = ADVANCED_FACE ( 'NONE', ( #1212 ), #19142, .T. ) ;
#19197 = VERTEX_POINT ( 'NONE', #6898 ) ;
#19198 = CARTESIAN_POINT ( 'NONE',  ( 22.79184847219999810, -10.23415548584000057, -3.837234280334999692 ) ) ;
#19199 = CARTESIAN_POINT ( 'NONE',  ( -0.2273504397345396943, 12.80486570122317680, -6.661112331329158032 ) ) ;
#19200 = AXIS2_PLACEMENT_3D ( 'NONE', #3020, #6759, #8836 ) ;
#19201 = CARTESIAN_POINT ( 'NONE',  ( -11.99999999434999864, 6.999999994347000154, 4.083276180409999442E-09 ) ) ;
#19202 = CIRCLE ( 'NONE', #23455, 4.649999999999999467 ) ;
#19203 = CARTESIAN_POINT ( 'NONE',  ( -19.35893705290999733, -9.828989445528000246, 3.502754984265999738 ) ) ;
#19204 = CARTESIAN_POINT ( 'NONE',  ( 23.41677564524290744, 34.01856778792605240, -115.0195023120000002 ) ) ;
#19205 = DIRECTION ( 'NONE',  ( -1.000000000000000000, 0.000000000000000000, 0.000000000000000000 ) ) ;
#19206 = VERTEX_POINT ( 'NONE', #21687 ) ;
#19207 = CARTESIAN_POINT ( 'NONE',  ( -17.04240246313371188, -1.782570974809130293, -10.26454133355910336 ) ) ;
#19208 = CARTESIAN_POINT ( 'NONE',  ( -3.999999999999999112, 29.94682129341587995, -0.9440428258622635127 ) ) ;
#19209 = CONICAL_SURFACE ( 'NONE', #10722, 7.249999994833000727, 0.7853981633972997312 ) ;
#19210 = CARTESIAN_POINT ( 'NONE',  ( -0.4182960933211564702, 28.60509501925429277, 2.130789602436458541 ) ) ;
#19211 = AXIS2_PLACEMENT_3D ( 'NONE', #16908, #11358, #82 ) ;
#19212 = DIRECTION ( 'NONE',  ( 1.000000000000000000, 0.000000000000000000, 0.000000000000000000 ) ) ;
#19213 = ORIENTED_EDGE ( 'NONE', *, *, #1811, .F. ) ;
#19214 = B_SPLINE_CURVE_WITH_KNOTS ( 'NONE', 3,
 ( #1367, #4766, #4886, #16254, #12274, #16121, #3075, #17849, #6935, #14331, #5130, #19898, #23647, #7054, #14437, #21832, #9460, #3657, #7160, #18316, #5355, #9224, #11285, #3546, #12746, #7277, #1611, #1955, #5702, #14670, #5587, #12968, #18549, #14779, #9108, #5821, #18662, #8997, #4005, #20487, #23871, #16367, #3895, #20364, #3774, #20138, #23757, #7512, #2069, #16603, #9341, #16480, #12855, #11043, #14551, #16834, #10930, #20252, #21945, #18427, #22413, #22065, #238, #1718, #1837, #13, #7397, #5473, #22175, #11162, #16714, #13088, #125, #14896, #7641, #22286, #15014, #13204, #20596, #18210, #9811, #18771, #4251, #13316, #19258, #22997, #20839, #17196, #591, #11403, #7760, #6048, #21073, #2181, #9931, #19009, #15609, #20714, #22879 ),
 .UNSPECIFIED., .F., .F.,
 ( 4, 2, 2, 2, 1, 1, 2, 2, 1, 1, 1, 2, 2, 2, 2, 1, 1, 2, 1, 1, 1, 2, 2, 2, 2, 2, 1, 1, 1, 1, 1, 2, 2, 2, 2, 2, 2, 2, 1, 1, 1, 1, 1, 2, 2, 2, 2, 2, 2, 2, 2, 1, 1, 1, 1, 1, 2, 2, 2, 2, 2, 4 ),
 ( 0.000000000000000000, 0.03125000000005528911, 0.06250000000011057821, 0.07812500000013818113, 0.08203125000014512003, 0.08300781250014672985, 0.08325195312514714618, 0.08337402343764720170, 0.08349609375014727108, 0.08398437500014754864, 0.08593750000014858947, 0.09375000000015272505, 0.1250000000001691147, 0.1562500000001855460, 0.1640625000001895983, 0.1660156250001906530, 0.1665039062501909306, 0.1666259765626908473, 0.1667480468751907918, 0.1669921875001907086, 0.1679687500001903755, 0.1718750000001889877, 0.1875000000001834088, 0.2187500000001722789, 0.2343750000001667000, 0.2421875000001639244, 0.2460937500001625367, 0.2480468750001618428, 0.2490234375001615097, 0.2495117187501613432, 0.2497558593751612599, 0.2498779296876612321, 0.2500000000001612044, 0.3125000000001456057, 0.3750000000001300071, 0.4375000000001144085, 0.4687500000001066369, 0.4843750000001026956, 0.4921875000001008083, 0.4960937500000998090, 0.4980468750000993650, 0.4990234375000991429, 0.4995117187500989764, 0.4997558593750989209, 0.5000000000000988098, 0.5312500000000929257, 0.5625000000000869305, 0.6250000000000750511, 0.6875000000000631717, 0.7187500000000571765, 0.7343750000000541789, 0.7421875000000526246, 0.7460937500000519584, 0.7480468750000516254, 0.7490234375000514033, 0.7495117187500512923, 0.7497558593750511813, 0.7500000000000510703, 0.8125000000000383027, 0.8750000000000255351, 0.9375000000000127676, 1.000000000000000000 ),
 .UNSPECIFIED. ) ;
#19215 = DIRECTION ( 'NONE',  ( 0.000000000000000000, 1.000000000000000000, 0.000000000000000000 ) ) ;
#19216 = CONICAL_SURFACE ( 'NONE', #6461, 4.309401076758999416, 1.119376321708719590 ) ;
#19217 = CARTESIAN_POINT ( 'NONE',  ( 16.62693924930999856, 10.62505432564000074, 1.551621659364999850 ) ) ;
#19218 = CARTESIAN_POINT ( 'NONE',  ( -14.56155220878999046, -7.925308545561296825, -4.456233346637926473 ) ) ;
#19219 = CARTESIAN_POINT ( 'NONE',  ( -18.20383756955000010, 6.087427736527000199, 9.656242520863001388 ) ) ;
#19220 = DIRECTION ( 'NONE',  ( 0.000000000000000000, 1.000000000000000000, 0.000000000000000000 ) ) ;
#19221 = CARTESIAN_POINT ( 'NONE',  ( 13.16181994525999954, 0.8615620839388999919, -9.360004375220999151 ) ) ;
#19222 = CARTESIAN_POINT ( 'NONE',  ( -4.000000000000000000, 26.50000000000001066, -0.1857058784358549819 ) ) ;
#19223 = CARTESIAN_POINT ( 'NONE',  ( 0.000000000000000000, 24.29999999999999716, -4.749999999999970690 ) ) ;
#19224 = CARTESIAN_POINT ( 'NONE',  ( 24.91638881842000330, 0.3555708854531000607, 10.32200993542000056 ) ) ;
#19225 = CARTESIAN_POINT ( 'NONE',  ( -1.236362846991004183, 26.50000008335574719, -2.171602059085420589 ) ) ;
#19226 = ORIENTED_EDGE ( 'NONE', *, *, #13530, .T. ) ;
#19227 = CARTESIAN_POINT ( 'NONE',  ( -2.143920584830219411, 13.91597717198021478, 5.737536879300400905 ) ) ;
#19228 = CARTESIAN_POINT ( 'NONE',  ( -2.447990496630999768, 26.39000240010000198, -1.500144717171000064 ) ) ;
#19229 = AXIS2_PLACEMENT_3D ( 'NONE', #14621, #5431, #12580 ) ;
#19230 = CARTESIAN_POINT ( 'NONE',  ( -3.916368311430999505, 12.23844822715000369, 2.656827315156998548 ) ) ;
#19231 = CARTESIAN_POINT ( 'NONE',  ( 2.144482848013529619, 29.02030102469518980, -0.2779858083291430471 ) ) ;
#19232 = CARTESIAN_POINT ( 'NONE',  ( -24.57378270132000253, -9.262129720473000205, -5.482658259817999813 ) ) ;
#19233 = CONICAL_SURFACE ( 'NONE', #20027, 13.20532192316000142, 0.7853981633972997312 ) ;
#19234 = DIRECTION ( 'NONE',  ( -1.167437209404000066E-09, -4.744820243581140101E-20, -1.000000000000000000 ) ) ;
#19235 = ORIENTED_EDGE ( 'NONE', *, *, #20043, .T. ) ;
#19236 = ADVANCED_FACE ( 'NONE', ( #13924, #14048 ), #5098, .F. ) ;
#19237 = CARTESIAN_POINT ( 'NONE',  ( 15.18224770046331606, -7.245781551128942510, -5.568249303537384343 ) ) ;
#19238 = AXIS2_PLACEMENT_3D ( 'NONE', #10384, #21286, #1044 ) ;
#19239 = CARTESIAN_POINT ( 'NONE',  ( 8.124934037954998800, 1.125145054518999965E-14, 0.000000000000000000 ) ) ;
#19240 = LINE ( 'NONE', #19370, #14596 ) ;
#19241 = CARTESIAN_POINT ( 'NONE',  ( -1.600067560738497097, 6.964050391730369327, 0.7113046981209643072 ) ) ;
#19242 = CARTESIAN_POINT ( 'NONE',  ( -7.500000000000000000, 22.00000000000000000, -1.000000000000000000 ) ) ;
#19243 = CARTESIAN_POINT ( 'NONE',  ( -14.82384736926000102, 5.788590216149999357, -9.100136119003000346 ) ) ;
#19244 = AXIS2_PLACEMENT_3D ( 'NONE', #17804, #17550, #17674 ) ;
#19245 = CIRCLE ( 'NONE', #7650, 2.100000000000000089 ) ;
#19246 = CARTESIAN_POINT ( 'NONE',  ( 11.39231375731000107, -8.729484032481000355, -2.472142458034000345 ) ) ;
#19247 = CARTESIAN_POINT ( 'NONE',  ( -9.000000000000000000, 19.50000000000000000, -5.000000000000000000 ) ) ;
#19248 = ORIENTED_EDGE ( 'NONE', *, *, #9835, .T. ) ;
#19249 = PLANE ( 'NONE',  #23155 ) ;
#19250 = CARTESIAN_POINT ( 'NONE',  ( -1.480915476144999854, 31.13702747345000077, -2.141804436516000276 ) ) ;
#19251 = B_SPLINE_CURVE_WITH_KNOTS ( 'NONE', 3,
 ( #20392, #18686, #11067, #2092, #6407, #3797, #17438, #16626, #20273, #261, #11191, #13229, #9600, #4477, #11865, #4032, #11426, #710 ),
 .UNSPECIFIED., .F., .F.,
 ( 4, 2, 2, 2, 2, 2, 2, 2, 4 ),
 ( 0.000000000000000000, 0.1249999999999999722, 0.2500000000000000000, 0.3750000000000000000, 0.5000000000000001110, 0.6250000000000001110, 0.7500000000000000000, 0.8750000000000000000, 1.000000000000000000 ),
 .UNSPECIFIED. ) ;
#19252 = CARTESIAN_POINT ( 'NONE',  ( -2.261090823039999975, 23.59650489110000038, 0.2002084280613000145 ) ) ;
#19253 = CARTESIAN_POINT ( 'NONE',  ( 2.113792074058734816, 13.90978049634387936, -5.748768854935037531 ) ) ;
#19254 = VERTEX_POINT ( 'NONE', #8851 ) ;
#19255 = CARTESIAN_POINT ( 'NONE',  ( -4.023636228000000870, 13.98888312590999661, -4.533167282472001069 ) ) ;
#19256 = DIRECTION ( 'NONE',  ( -0.7071067811865465735, 0.7071067811865465735, -5.135208680714336970E-08 ) ) ;
#19257 = CARTESIAN_POINT ( 'NONE',  ( 1.867682715928999926, 29.47894642224000350, -2.012571957185000038 ) ) ;
#19258 = CARTESIAN_POINT ( 'NONE',  ( 14.40516388438136985, -4.484488855952614372, 7.850264337849301555 ) ) ;
#19259 = CARTESIAN_POINT ( 'NONE',  ( -6.651120061331225131, 15.37734650507915113, -1.642905757035629577 ) ) ;
#19260 = DIRECTION ( 'NONE',  ( 0.000000000000000000, 0.000000000000000000, 1.000000000000000000 ) ) ;
#19261 = CARTESIAN_POINT ( 'NONE',  ( -21.58741243917332753, -2.414574286862336550, -8.985197089948746552 ) ) ;
#19262 = CARTESIAN_POINT ( 'NONE',  ( -2.184465970885646424, 29.76753006952333180, -1.259047450927245126 ) ) ;
#19263 = ORIENTED_EDGE ( 'NONE', *, *, #22523, .F. ) ;
#19264 = DIRECTION ( 'NONE',  ( 0.000000000000000000, -0.9999173538268769645, 0.01285634146465969990 ) ) ;
#19265 = CARTESIAN_POINT ( 'NONE',  ( 0.9658031675207989775, 24.49999999999999645, -2.222895075323709779 ) ) ;
#19266 = ORIENTED_EDGE ( 'NONE', *, *, #9098, .T. ) ;
#19267 = ADVANCED_FACE ( 'NONE', ( #21799 ), #19941, .F. ) ;
#19268 = PRODUCT_DEFINITION_SHAPE ( 'NONE', 'NONE',  #6191 ) ;
#19269 = CARTESIAN_POINT ( 'NONE',  ( 0.000000000000000000, 14.90000000000000036, -4.724999999995984190 ) ) ;
#19270 = CARTESIAN_POINT ( 'NONE',  ( 2.434931691670792819, 28.60086340285666751, 0.6543697108981857413 ) ) ;
#19271 = CARTESIAN_POINT ( 'NONE',  ( 3.217986197202229448, 13.15087042456258537, 5.950358584322657407 ) ) ;
#19272 = CARTESIAN_POINT ( 'NONE',  ( 17.47883835214000214, -6.259200876991000584, 9.163567223394000649 ) ) ;
#19273 = CARTESIAN_POINT ( 'NONE',  ( -20.92363501368665979, 8.282032949706003677, 4.165695112817996204 ) ) ;
#19274 = CONICAL_SURFACE ( 'NONE', #21975, 9.152445778720998959, 0.02565634000431304615 ) ;
#19275 = DIRECTION ( 'NONE',  ( 0.000000000000000000, 1.000000000000000000, 0.000000000000000000 ) ) ;
#19276 = ORIENTED_EDGE ( 'NONE', *, *, #4448, .T. ) ;
#19277 = ORIENTED_EDGE ( 'NONE', *, *, #18513, .T. ) ;
#19278 = CARTESIAN_POINT ( 'NONE',  ( -14.00000000000000355, -4.688626905535442368, -8.566863040657263895 ) ) ;
#19279 = AXIS2_PLACEMENT_3D ( 'NONE', #8121, #8236, #13309 ) ;
#19280 = CARTESIAN_POINT ( 'NONE',  ( -1.750000000000000000, 7.000000000000000000, 0.000000000000000000 ) ) ;
#19281 = DIRECTION ( 'NONE',  ( 0.000000000000000000, 1.000000000000000000, 0.000000000000000000 ) ) ;
#19282 =( BOUNDED_SURFACE ( )  B_SPLINE_SURFACE ( 3, 3, ( 
 ( #10128, #19822, #10376, #3118, #13876, #4807, #16041, #21279, #6728, #19339, #1289, #14243, #1168, #12192, #4689, #19582, #10619, #2988, #21639, #2747, #19459, #12438, #17517, #1037, #8439, #17765, #910 ),
 ( #3236, #15920, #23314, #14120, #8312, #15678, #4927, #1408, #12314, #8802, #10503, #22949, #23065, #6364, #4562, #11952, #6495, #12074, #6974, #1643, #14590, #1533, #5399, #22100, #16401, #14478, #10735 ),
 ( #1880, #14707, #21987, #11083, #5510, #23681, #9032, #16288, #23792, #14364, #18468, #23911, #3358, #12785, #21870, #5169, #21755, #23565, #7321, #20173, #9149, #18128, #12887, #18349, #20288, #12670, #12552 ),
 ( #3692, #7201, #16525, #20056, #19937, #9267, #7089, #8921, #5280, #1760, #3472, #10856, #16644, #18239, #16165, #3581, #10965, #2947, #17725, #16122, #19541, #23272, #996, #10695, #1244, #17964, #4767 ),
 ( #23392, #12275, #12033, #8634, #6810, #12513, #15883, #23523, #8397, #8524, #21234, #6686, #18086, #15764, #19899, #19416, #8885, #4887, #2828, #15997, #12401, #6936, #14332, #3076, #21473, #14203, #23153 ),
 ( #4646, #19787, #6574, #21600, #14079, #10463, #3315, #10578, #1368, #1491, #13957, #21721, #17602, #19662, #5132, #5016, #17850, #16255, #3195, #21351, #8758, #23648, #13833, #10208, #12152, #10335, #1125 ),
 ( #2070, #7278, #7513, #10931, #3437, #14671, #1612, #22287, #9342, #5703, #22066, #14780, #14897, #23759, #18429, #3658, #16604, #1719, #5356, #20253, #8998, #20015, #16368, #21833, #1956, #5474, #10821 ) ),
 .UNSPECIFIED., .F., .F., .T. ) 
 B_SPLINE_SURFACE_WITH_KNOTS ( ( 4, 3, 4 ),
 ( 4, 1, 1, 1, 1, 1, 1, 1, 1, 1, 1, 1, 1, 1, 1, 1, 1, 1, 1, 1, 1, 1, 1, 1, 4 ),
 ( 0.000000000000000000, 1.000000000000000000, 2.000000000000000000 ),
 ( 0.4898034299706000017, 0.4943545979319000083, 0.5111317270519999401, 0.5298150905820000478, 0.5506159615357999471, 0.5738885039238000862, 0.6000497485708999879, 0.6296087238595999835, 0.6631460577478999197, 0.6990545679290000036, 0.7337557558452000306, 0.7651098038429999804, 0.7931348371437000333, 0.8181853307084000493, 0.8407431172970000199, 0.8611305378076999917, 0.8795824795753000025, 0.8963530464747999638, 0.9117079150094000717, 0.9258708385234000193, 0.9397608587919999978, 0.9542041168318999844, 0.9687118367007999664, 0.9836094246282999221, 0.9997243908991000350 ),
 .UNSPECIFIED. ) 
 GEOMETRIC_REPRESENTATION_ITEM ( )  RATIONAL_B_SPLINE_SURFACE ( (
 ( 1.293342249838999924, 1.293342249838999924, 1.293342249838999924, 1.293342249838999924, 1.293342249838999924, 1.293342249838999924, 1.293342249838999924, 1.293342249838999924, 1.293342249838999924, 1.293342249838999924, 1.293342249838999924, 1.293342249838999924, 1.293342249838999924, 1.293342249838999924, 1.293342249838999924, 1.293342249838999924, 1.293342249838999924, 1.293342249838999924, 1.293342249838999924, 1.293342249838999924, 1.293342249838999924, 1.293342249838999924, 1.293342249838999924, 1.293342249838999924, 1.293342249838999924, 1.293342249838999924, 1.293342249838999924),
 ( 0.9022192500537999926, 0.9022192500537999926, 0.9022192500537999926, 0.9022192500537999926, 0.9022192500537999926, 0.9022192500537999926, 0.9022192500537999926, 0.9022192500537999926, 0.9022192500537999926, 0.9022192500537999926, 0.9022192500537999926, 0.9022192500537999926, 0.9022192500537999926, 0.9022192500537999926, 0.9022192500537999926, 0.9022192500537999926, 0.9022192500537999926, 0.9022192500537999926, 0.9022192500537999926, 0.9022192500537999926, 0.9022192500537999926, 0.9022192500537999926, 0.9022192500537999926, 0.9022192500537999926, 0.9022192500537999926, 0.9022192500537999926, 0.9022192500537999926),
 ( 0.9022192500537999926, 0.9022192500537999926, 0.9022192500537999926, 0.9022192500537999926, 0.9022192500537999926, 0.9022192500537999926, 0.9022192500537999926, 0.9022192500537999926, 0.9022192500537999926, 0.9022192500537999926, 0.9022192500537999926, 0.9022192500537999926, 0.9022192500537999926, 0.9022192500537999926, 0.9022192500537999926, 0.9022192500537999926, 0.9022192500537999926, 0.9022192500537999926, 0.9022192500537999926, 0.9022192500537999926, 0.9022192500537999926, 0.9022192500537999926, 0.9022192500537999926, 0.9022192500537999926, 0.9022192500537999926, 0.9022192500537999926, 0.9022192500537999926),
 ( 1.293342249838999924, 1.293342249838999924, 1.293342249838999924, 1.293342249838999924, 1.293342249838999924, 1.293342249838999924, 1.293342249838999924, 1.293342249838999924, 1.293342249838999924, 1.293342249838999924, 1.293342249838999924, 1.293342249838999924, 1.293342249838999924, 1.293342249838999924, 1.293342249838999924, 1.293342249838999924, 1.293342249838999924, 1.293342249838999924, 1.293342249838999924, 1.293342249838999924, 1.293342249838999924, 1.293342249838999924, 1.293342249838999924, 1.293342249838999924, 1.293342249838999924, 1.293342249838999924, 1.293342249838999924),
 ( 0.9022192500537999926, 0.9022192500537999926, 0.9022192500537999926, 0.9022192500537999926, 0.9022192500537999926, 0.9022192500537999926, 0.9022192500537999926, 0.9022192500537999926, 0.9022192500537999926, 0.9022192500537999926, 0.9022192500537999926, 0.9022192500537999926, 0.9022192500537999926, 0.9022192500537999926, 0.9022192500537999926, 0.9022192500537999926, 0.9022192500537999926, 0.9022192500537999926, 0.9022192500537999926, 0.9022192500537999926, 0.9022192500537999926, 0.9022192500537999926, 0.9022192500537999926, 0.9022192500537999926, 0.9022192500537999926, 0.9022192500537999926, 0.9022192500537999926),
 ( 0.9022192500537999926, 0.9022192500537999926, 0.9022192500537999926, 0.9022192500537999926, 0.9022192500537999926, 0.9022192500537999926, 0.9022192500537999926, 0.9022192500537999926, 0.9022192500537999926, 0.9022192500537999926, 0.9022192500537999926, 0.9022192500537999926, 0.9022192500537999926, 0.9022192500537999926, 0.9022192500537999926, 0.9022192500537999926, 0.9022192500537999926, 0.9022192500537999926, 0.9022192500537999926, 0.9022192500537999926, 0.9022192500537999926, 0.9022192500537999926, 0.9022192500537999926, 0.9022192500537999926, 0.9022192500537999926, 0.9022192500537999926, 0.9022192500537999926),
 ( 1.293342249838999924, 1.293342249838999924, 1.293342249838999924, 1.293342249838999924, 1.293342249838999924, 1.293342249838999924, 1.293342249838999924, 1.293342249838999924, 1.293342249838999924, 1.293342249838999924, 1.293342249838999924, 1.293342249838999924, 1.293342249838999924, 1.293342249838999924, 1.293342249838999924, 1.293342249838999924, 1.293342249838999924, 1.293342249838999924, 1.293342249838999924, 1.293342249838999924, 1.293342249838999924, 1.293342249838999924, 1.293342249838999924, 1.293342249838999924, 1.293342249838999924, 1.293342249838999924, 1.293342249838999924) ) ) 
 REPRESENTATION_ITEM ( '' )  SURFACE ( )  );
#19283 = ORIENTED_EDGE ( 'NONE', *, *, #7026, .F. ) ;
#19284 = EDGE_CURVE ( 'NONE', #9908, #10857, #14125, .T. ) ;
#19285 = DIRECTION ( 'NONE',  ( -1.000000000000000000, 0.000000000000000000, 0.000000000000000000 ) ) ;
#19286 = CARTESIAN_POINT ( 'NONE',  ( 0.000000000000000000, 30.84509624898000268, 0.000000000000000000 ) ) ;
#19287 = CARTESIAN_POINT ( 'NONE',  ( 15.81878663761505166, -10.36539687577051261, 0.1259574713066463070 ) ) ;
#19288 = CONICAL_SURFACE ( 'NONE', #14260, 13.97499999999999964, 1.402900403544236729 ) ;
#19289 = CARTESIAN_POINT ( 'NONE',  ( -15.27343108650000048, 7.751837191927000603, -7.841115722439000457 ) ) ;
#19290 = DIRECTION ( 'NONE',  ( 0.000000000000000000, 0.000000000000000000, -1.000000000000000000 ) ) ;
#19291 = CARTESIAN_POINT ( 'NONE',  ( 8.124934037954998800, -14.44999999999999929, 0.000000000000000000 ) ) ;
#19292 = DIRECTION ( 'NONE',  ( 1.000000000000000000, 0.000000000000000000, 0.000000000000000000 ) ) ;
#19293 = ADVANCED_FACE ( 'NONE', ( #10545 ), #19507, .T. ) ;
#19294 = AXIS2_PLACEMENT_3D ( 'NONE', #9782, #20566, #22613 ) ;
#19295 = CARTESIAN_POINT ( 'NONE',  ( -2.044419059392999838, 29.44573095519140438, 0.6966517550941788706 ) ) ;
#19296 = ORIENTED_EDGE ( 'NONE', *, *, #1121, .F. ) ;
#19297 = CARTESIAN_POINT ( 'NONE',  ( -1.802597709787000069, 23.71057944035000276, 1.505962647774000018 ) ) ;
#19298 = CARTESIAN_POINT ( 'NONE',  ( -15.33118988585713360, 1.667259466958864955, -10.39754702251702767 ) ) ;
#19299 = VECTOR ( 'NONE', #11484, 1000.000000000000000 ) ;
#19300 = VERTEX_POINT ( 'NONE', #23614 ) ;
#19301 = EDGE_CURVE ( 'NONE', #16017, #10983, #20023, .T. ) ;
#19302 = DIRECTION ( 'NONE',  ( 0.000000000000000000, -1.000000000000000000, 0.000000000000000000 ) ) ;
#19303 = CARTESIAN_POINT ( 'NONE',  ( 6.274105421348001421, 13.70217340327999445, -0.0001422782095605998798 ) ) ;
#19304 = CLOSED_SHELL ( 'NONE', ( #2109, #1430, #4082, #17508, #19623, #571 ) ) ;
#19305 = CARTESIAN_POINT ( 'NONE',  ( 1.346439123301719665, 28.03198827073827459, 3.841100253455552060 ) ) ;
#19306 = CARTESIAN_POINT ( 'NONE',  ( 17.42999999999999972, 9.118569865760999704, 0.000000000000000000 ) ) ;
#19307 = CARTESIAN_POINT ( 'NONE',  ( 12.84468892131000040, 2.447276857699999919, 9.303608529293999396 ) ) ;
#19308 = EDGE_LOOP ( 'NONE', ( #16984, #7072, #3449 ) ) ;
#19309 = DIRECTION ( 'NONE',  ( -1.000000000000000000, 0.000000000000000000, 0.000000000000000000 ) ) ;
#19310 = FACE_BOUND ( 'NONE', #4046, .T. ) ;
#19311 = CARTESIAN_POINT ( 'NONE',  ( 0.000000000000000000, 24.65000000000000213, 0.000000000000000000 ) ) ;
#19312 = CIRCLE ( 'NONE', #14656, 2.750000000000000000 ) ;
#19313 = ORIENTED_EDGE ( 'NONE', *, *, #5257, .T. ) ;
#19314 = EDGE_CURVE ( 'NONE', #7294, #20019, #7019, .T. ) ;
#19315 = CARTESIAN_POINT ( 'NONE',  ( -14.00000000000000000, 1.396097351027999937E-14, 0.000000000000000000 ) ) ;
#19316 = CARTESIAN_POINT ( 'NONE',  ( 14.99328936713000004, -9.056039068417000237, 0.000000000000000000 ) ) ;
#19317 = CYLINDRICAL_SURFACE ( 'NONE', #9253, 4.750000000000000000 ) ;
#19318 = CARTESIAN_POINT ( 'NONE',  ( -23.50032910583999879, -5.270462733209999584, -7.631233524726999562 ) ) ;
#19320 = CARTESIAN_POINT ( 'NONE',  ( 18.42637794657805372, 9.567720008368787887, -4.137431501767250275 ) ) ;
#19319 = AXIS2_PLACEMENT_3D ( 'NONE', #8604, #12481, #19508 ) ;
#19321 = AXIS2_PLACEMENT_3D ( 'NONE', #8884, #10577, #8757 ) ;
#19322 = CARTESIAN_POINT ( 'NONE',  ( 12.00000000000000000, -7.836133899445423268, -6.030681244544030761 ) ) ;
#19323 = CARTESIAN_POINT ( 'NONE',  ( -14.50000017458758883, -10.95512910623405567, 6.025157725042295631 ) ) ;
#19324 = CARTESIAN_POINT ( 'NONE',  ( 24.49298667129999885, -10.14947584299000027, 2.979949436719000033 ) ) ;
#19325 = FACE_OUTER_BOUND ( 'NONE', #15860, .T. ) ;
#19326 = CIRCLE ( 'NONE', #2635, 1.399999999999999911 ) ;
#19327 = CYLINDRICAL_SURFACE ( 'NONE', #6764, 2.500000000000000000 ) ;
#19328 = DIRECTION ( 'NONE',  ( 0.000000000000000000, 0.000000000000000000, -1.000000000000000000 ) ) ;
#19329 = CARTESIAN_POINT ( 'NONE',  ( -1.951811984317841642, 30.14747925604160983, -0.9252638563299733221 ) ) ;
#19330 = ORIENTED_EDGE ( 'NONE', *, *, #7908, .F. ) ;
#19331 = CARTESIAN_POINT ( 'NONE',  ( 22.59859753864000353, -10.40165104099999915, 3.339338359392999944 ) ) ;
#19332 = CARTESIAN_POINT ( 'NONE',  ( -2.860127424524721462, 13.08059937058052924, -6.101802095341746224 ) ) ;
#19333 = CARTESIAN_POINT ( 'NONE',  ( 24.50000000000000000, 0.000000000000000000, 0.000000000000000000 ) ) ;
#19334 = AXIS2_PLACEMENT_3D ( 'NONE', #17087, #11530, #485 ) ;
#19335 = EDGE_CURVE ( 'NONE', #11502, #19694, #12366, .T. ) ;
#19336 = CARTESIAN_POINT ( 'NONE',  ( -20.51039254048601279, 3.918938775750210102, -9.746684010221523309 ) ) ;
#19337 = CARTESIAN_POINT ( 'NONE',  ( 4.835696606763119298, 14.67450102544439794, 3.769838936156646447 ) ) ;
#19338 = EDGE_CURVE ( 'NONE', #9790, #12389, #23011, .T. ) ;
#19339 = CARTESIAN_POINT ( 'NONE',  ( 2.436990620365000471, 11.77112358195999775, -4.345572479020002987 ) ) ;
#19340 = VERTEX_POINT ( 'NONE', #3403 ) ;
#19341 = CARTESIAN_POINT ( 'NONE',  ( -19.02410030640447758, -7.225764994020523524, -7.707796388380748986 ) ) ;
#19342 = DIRECTION ( 'NONE',  ( -1.000000000000000000, 0.000000000000000000, 0.000000000000000000 ) ) ;
#19343 = VECTOR ( 'NONE', #6107, 999.9999999999998863 ) ;
#19344 = CARTESIAN_POINT ( 'NONE',  ( -1.726962967392345671, 27.54490368590698779, -1.364955284461023322 ) ) ;
#19345 = PRODUCT_CONTEXT ( 'NONE', #3108, 'mechanical' ) ;
#19346 = ORIENTED_EDGE ( 'NONE', *, *, #15585, .T. ) ;
#19347 = VERTEX_POINT ( 'NONE', #10785 ) ;
#19348 = ADVANCED_FACE ( 'NONE', ( #3625 ), #5325, .T. ) ;
#19349 = CARTESIAN_POINT ( 'NONE',  ( 16.80728936713000365, -9.102589883624000677, 0.000000000000000000 ) ) ;
#19350 = ADVANCED_FACE ( 'NONE', ( #11369, #1803 ), #11008, .T. ) ;
#19351 = CARTESIAN_POINT ( 'NONE',  ( 18.60131424931000055, 8.248882947719001990, 6.955037127929000640 ) ) ;
#19352 = CARTESIAN_POINT ( 'NONE',  ( -20.20485756376000097, 10.40668476090000105, 3.922866990116000263 ) ) ;
#19353 = CARTESIAN_POINT ( 'NONE',  ( -17.66049696303999994, -8.440406808323999144, -6.840409896643000920 ) ) ;
#19354 = CARTESIAN_POINT ( 'NONE',  ( 0.000000000000000000, 20.10000000000000142, 0.000000000000000000 ) ) ;
#19355 = CARTESIAN_POINT ( 'NONE',  ( 18.03681994525999954, -9.876911530946999918, 3.071220598218000308 ) ) ;
#19356 = CARTESIAN_POINT ( 'NONE',  ( -2.189594054297049119, 28.61899650445837295, 0.2575912915343336329 ) ) ;
#19357 = CARTESIAN_POINT ( 'NONE',  ( -1.259047450927242018, 26.76753006952333180, 2.184465970885648201 ) ) ;
#19358 = CARTESIAN_POINT ( 'NONE',  ( 0.000000000000000000, 31.00000000000000000, 0.000000000000000000 ) ) ;
#19359 = CARTESIAN_POINT ( 'NONE',  ( 24.39431354042982747, 9.829649394705615606, 2.587219325858395311E-05 ) ) ;
#19360 = VERTEX_POINT ( 'NONE', #14520 ) ;
#19361 = CARTESIAN_POINT ( 'NONE',  ( 0.005043638803689440113, 13.69078929351160134, 6.125306092024061400 ) ) ;
#19362 = CARTESIAN_POINT ( 'NONE',  ( -2.153772461420000006, 28.71413313895000030, 1.206163983883000057 ) ) ;
#19363 = CARTESIAN_POINT ( 'NONE',  ( -4.723653023056002986, 12.53637152982000913, 0.1248203372519999244 ) ) ;
#19364 = CARTESIAN_POINT ( 'NONE',  ( -19.54666243917331769, 4.619757582330495715, -8.015095742238548482 ) ) ;
#19365 = CARTESIAN_POINT ( 'NONE',  ( -14.53474671855800793, 0.6128746787797743067, -9.025483422738085793 ) ) ;
#19366 = CARTESIAN_POINT ( 'NONE',  ( -19.57601527871000258, -10.43905349783999981, -0.1441279127309000041 ) ) ;
#19367 = CARTESIAN_POINT ( 'NONE',  ( 23.99062354302999722, 7.716878364870000340, 11.63397459621999985 ) ) ;
#19368 = ORIENTED_EDGE ( 'NONE', *, *, #936, .T. ) ;
#19369 = CARTESIAN_POINT ( 'NONE',  ( 4.143372994309425295, 12.32180263635245687, 2.404628968344424855 ) ) ;
#19370 = CARTESIAN_POINT ( 'NONE',  ( 0.000000000000000000, 30.84509624898000268, -2.154903751016000069 ) ) ;
#19371 = CARTESIAN_POINT ( 'NONE',  ( -0.6522852588204888225, 6.808683197727685155, 1.625598361106043166 ) ) ;
#19372 = DIRECTION ( 'NONE',  ( 0.000000000000000000, -1.000000000000000000, 0.000000000000000000 ) ) ;
#19373 = CARTESIAN_POINT ( 'NONE',  ( 2.184465970885644648, 27.10086340285666751, -1.259047450927249345 ) ) ;
#19374 = DIRECTION ( 'NONE',  ( 0.000000000000000000, 1.000000000000000000, 0.000000000000000000 ) ) ;
#19375 = CARTESIAN_POINT ( 'NONE',  ( 18.08325125730999972, 1.019414021290000028, 9.192347282599000025 ) ) ;
#19376 = CARTESIAN_POINT ( 'NONE',  ( 24.15736593520906794, 5.143174366503609818, 12.50000000000000355 ) ) ;
#19377 = ORIENTED_EDGE ( 'NONE', *, *, #7181, .T. ) ;
#19378 = CARTESIAN_POINT ( 'NONE',  ( -22.28593252662366808, -4.096005354656629294, 8.307274234526197176 ) ) ;
#19379 = CARTESIAN_POINT ( 'NONE',  ( 2.068822368684000157, 29.35017502063999828, -1.771798175640999951 ) ) ;
#19380 = CARTESIAN_POINT ( 'NONE',  ( 1.883643770067999990, 23.87661750703000152, -1.956741025826999936 ) ) ;
#19381 = CARTESIAN_POINT ( 'NONE',  ( 3.348931919835092863, 14.23418124123950612, -5.129098008807517317 ) ) ;
#19382 = ORIENTED_EDGE ( 'NONE', *, *, #8976, .T. ) ;
#19383 = CARTESIAN_POINT ( 'NONE',  ( 0.6016956921910996403, 12.73580660312999946, -6.459985624991999131 ) ) ;
#19384 = CARTESIAN_POINT ( 'NONE',  ( 19.42644257295000187, -9.760492247572999602, 5.443783144978000088 ) ) ;
#19385 = CARTESIAN_POINT ( 'NONE',  ( 1.772081371289000007, 29.26351976544000166, 2.097239190856999613 ) ) ;
#19386 = DIRECTION ( 'NONE',  ( -1.000000000000000000, 0.000000000000000000, 0.000000000000000000 ) ) ;
#19387 = CARTESIAN_POINT ( 'NONE',  ( 16.73383172034440136, 7.986707523212354332, 6.697168222554745753 ) ) ;
#19388 = DIRECTION ( 'NONE',  ( 0.000000000000000000, 0.000000000000000000, -1.000000000000000000 ) ) ;
#19389 = DIRECTION ( 'NONE',  ( 0.9996708941621516020, 0.02565352539211874019, 0.000000000000000000 ) ) ;
#19390 = CARTESIAN_POINT ( 'NONE',  ( -24.47970833437427629, -10.31330985779443488, 7.136763535896974986 ) ) ;
#19391 = VERTEX_POINT ( 'NONE', #13172 ) ;
#19392 = CARTESIAN_POINT ( 'NONE',  ( 19.05233531832000082, -1.887707665395999879, 10.26617185442000135 ) ) ;
#19393 = CARTESIAN_POINT ( 'NONE',  ( 11.29022434644563866, -9.635153832086475134, 8.311371697137628800 ) ) ;
#19394 = ORIENTED_EDGE ( 'NONE', *, *, #22393, .T. ) ;
#19395 = CARTESIAN_POINT ( 'NONE',  ( -0.7596549267136000205, 25.82419530016000309, 2.629617744858999906 ) ) ;
#19396 = DIRECTION ( 'NONE',  ( 1.000000000000000000, 0.000000000000000000, 0.000000000000000000 ) ) ;
#19397 = CARTESIAN_POINT ( 'NONE',  ( -0.4132613886251360058, 12.80949096665309028, 6.652112558386988006 ) ) ;
#19398 = CARTESIAN_POINT ( 'NONE',  ( 14.23072219092999902, -10.36232653785000046, -3.715438785038000180 ) ) ;
#19399 = CARTESIAN_POINT ( 'NONE',  ( -20.41853216811167826, -5.563930387130748834, 7.399052236490962109 ) ) ;
#19400 = CARTESIAN_POINT ( 'NONE',  ( 24.49999999999999289, -0.5123787730663437179, -12.50000000000000000 ) ) ;
#19401 = VERTEX_POINT ( 'NONE', #9310 ) ;
#19402 = VERTEX_POINT ( 'NONE', #20561 ) ;
#19403 = CARTESIAN_POINT ( 'NONE',  ( 1.999167105995457216, 30.15086340285667177, 1.536366799937278760 ) ) ;
#19404 = DIRECTION ( 'NONE',  ( 1.000000000000000000, 0.000000000000000000, 0.000000000000000000 ) ) ;
#19405 = CARTESIAN_POINT ( 'NONE',  ( 0.000000000000000000, 15.05000017415440006, 0.000000000000000000 ) ) ;
#19406 = VERTEX_POINT ( 'NONE', #22374 ) ;
#19407 = CARTESIAN_POINT ( 'NONE',  ( -22.34454660583000063, -8.644092610980999680, 4.380640856105999958 ) ) ;
#19408 = CARTESIAN_POINT ( 'NONE',  ( 1.699999998837999904, 12.90000000000000036, -1.053565373074999867 ) ) ;
#19409 = CARTESIAN_POINT ( 'NONE',  ( 20.90683333333332072, 8.045594964192355647, -4.637336234581411532 ) ) ;
#19410 = CARTESIAN_POINT ( 'NONE',  ( 14.97268632185512516, 10.13434347433388893, 2.013073180653659922 ) ) ;
#19411 = B_SPLINE_CURVE_WITH_KNOTS ( 'NONE', 3,
 ( #11475, #18497, #5652, #20316, #20670, #7718 ),
 .UNSPECIFIED., .F., .F.,
 ( 4, 1, 1, 4 ),
 ( 0.000000000000000000, 0.3333333333333000081, 0.6666666666667000474, 1.000000000000000000 ),
 .UNSPECIFIED. ) ;
#19412 = CARTESIAN_POINT ( 'NONE',  ( -14.94614617458000083, 10.86682107414999976, -1.813459502821000102 ) ) ;
#19413 = ADVANCED_FACE ( 'NONE', ( #21912, #3976 ), #14978, .T. ) ;
#19414 = CARTESIAN_POINT ( 'NONE',  ( -2.355489761170999952, 29.22512865352000233, 0.05855059890257999916 ) ) ;
#19415 = CARTESIAN_POINT ( 'NONE',  ( -19.96961337912605217, 2.058113591641633100, 10.28927962370347693 ) ) ;
#19416 = CARTESIAN_POINT ( 'NONE',  ( -2.677512966247001192, 11.87892984889000303, -3.907459004194998808 ) ) ;
#19417 = CARTESIAN_POINT ( 'NONE',  ( -13.84895371062999914, -11.26122607477999971, -0.8537354506236000118 ) ) ;
#19418 = CIRCLE ( 'NONE', #21743, 2.899999999999999911 ) ;
#19419 = CARTESIAN_POINT ( 'NONE',  ( -2.067964573227998315, 29.44117847301367874, 0.6230106560362024259 ) ) ;
#19420 = VERTEX_POINT ( 'NONE', #12932 ) ;
#19421 = CARTESIAN_POINT ( 'NONE',  ( 2.183938845894000114, 24.79402139891000090, -0.09232374713782000308 ) ) ;
#19422 = CARTESIAN_POINT ( 'NONE',  ( -14.98391979967643728, 10.15505035706891945, -2.115929780933073712 ) ) ;
#19423 = VERTEX_POINT ( 'NONE', #7479 ) ;
#19424 = CARTESIAN_POINT ( 'NONE',  ( -12.00000000000000000, 1.371604415045000054E-14, 0.000000000000000000 ) ) ;
#19425 = CARTESIAN_POINT ( 'NONE',  ( 5.701809914176997118, 14.61127657005998159, -2.263870544078999014 ) ) ;
#19426 = ADVANCED_FACE ( 'NONE', ( #18285 ), #22233, .T. ) ;
#19427 = CARTESIAN_POINT ( 'NONE',  ( 12.00000000000000178, 0.2542798753839149439, -8.980062289379773688 ) ) ;
#19428 = CIRCLE ( 'NONE', #18271, 3.100000000000000089 ) ;
#19429 = DIRECTION ( 'NONE',  ( 0.000000000000000000, 1.000000000000000000, 0.000000000000000000 ) ) ;
#19430 = CARTESIAN_POINT ( 'NONE',  ( 12.95437642131000011, -1.177851786523999911, 9.550625374955998836 ) ) ;
#19431 = EDGE_LOOP ( 'NONE', ( #327, #5694, #7204 ) ) ;
#19432 = CARTESIAN_POINT ( 'NONE',  ( -10.62189649291999949, -7.518817411396999439, -12.41885835890000145 ) ) ;
#19433 = DIRECTION ( 'NONE',  ( 0.000000000000000000, 1.000000000000000000, 0.000000000000000000 ) ) ;
#19434 = FILL_AREA_STYLE_COLOUR ( '', #285 ) ;
#19435 = B_SPLINE_CURVE_WITH_KNOTS ( 'NONE', 3,
 ( #20955, #4360, #2538, #19126, #17315, #13675, #21070, #4483, #6778, #12367, #15852, #19754, #19631, #5099 ),
 .UNSPECIFIED., .F., .F.,
 ( 4, 2, 2, 2, 2, 2, 4 ),
 ( 0.000000000000000000, 0.2500000000000000555, 0.3750000000000001665, 0.5000000000000002220, 0.6250000000000003331, 0.7500000000000004441, 1.000000000000000000 ),
 .UNSPECIFIED. ) ;
#19436 = EDGE_LOOP ( 'NONE', ( #56, #17537, #16843, #8357, #2816 ) ) ;
#19437 = CARTESIAN_POINT ( 'NONE',  ( 4.000000000000000000, 26.20000000000000284, -2.309401076759000304 ) ) ;
#19438 = CARTESIAN_POINT ( 'NONE',  ( 11.85409292833919714, 13.07924560383835200, 2.346130611937419452 ) ) ;
#19439 = DIRECTION ( 'NONE',  ( -0.000000000000000000, -1.000000000000000000, -0.000000000000000000 ) ) ;
#19440 = CONICAL_SURFACE ( 'NONE', #21779, 4.674999969225999585, 0.7853981633972997312 ) ;
#19441 = CARTESIAN_POINT ( 'NONE',  ( -12.49032736094479290, 6.973667062827473728, -5.693396044204937390 ) ) ;
#19442 = CARTESIAN_POINT ( 'NONE',  ( 16.27407586645121640, -0.09550682843461062721, -10.36543807879250956 ) ) ;
#19443 = CARTESIAN_POINT ( 'NONE',  ( 11.99999999999999822, -8.311814688850533983, -5.425963580743933257 ) ) ;
#19444 = ADVANCED_FACE ( 'NONE', ( #2152, #5789 ), #20448, .T. ) ;
#19445 = PLANE ( 'NONE',  #22290 ) ;
#19446 = CARTESIAN_POINT ( 'NONE',  ( 22.43704471257999700, 0.6835673466426999134, 11.23757390362000130 ) ) ;
#19447 = CARTESIAN_POINT ( 'NONE',  ( -0.4393762720424915225, 26.31534065533142552, 4.365128144578328317 ) ) ;
#19448 = CARTESIAN_POINT ( 'NONE',  ( 1.839173991642404138, 26.50000000000000355, 3.556954554355651776 ) ) ;
#19449 = CARTESIAN_POINT ( 'NONE',  ( 12.50898080071999985, 6.466862063081999956, -12.35567184454000156 ) ) ;
#19450 = CARTESIAN_POINT ( 'NONE',  ( -1.801854931646215796, 30.12917346635381222, -1.194674909710682575 ) ) ;
#19451 = ORIENTED_EDGE ( 'NONE', *, *, #16904, .T. ) ;
#19452 = CARTESIAN_POINT ( 'NONE',  ( 23.17835033931999789, 1.382018527918999817, -10.85292862796000080 ) ) ;
#19453 = CARTESIAN_POINT ( 'NONE',  ( 23.70405517126128458, 5.919522458329209869, -8.807685190096355754 ) ) ;
#19454 = CARTESIAN_POINT ( 'NONE',  ( -1.222626843528073604, 23.61650379099185670, -1.727787963671160165 ) ) ;
#19455 = CARTESIAN_POINT ( 'NONE',  ( -2.217776889426126274, 24.45298137823828810, 0.3983591268742258107 ) ) ;
#19456 = CARTESIAN_POINT ( 'NONE',  ( 4.849422839656808648, 14.57858754772911603, 3.779267820556795332 ) ) ;
#19457 = EDGE_CURVE ( 'NONE', #6384, #23625, #14146, .T. ) ;
#19458 = CONICAL_SURFACE ( 'NONE', #19855, 12.68487026514999982, 0.6105562205522639951 ) ;
#19459 = CARTESIAN_POINT ( 'NONE',  ( -4.488611054452003479, 12.34747560695998558, -2.085835349536002248 ) ) ;
#19460 = ORIENTED_EDGE ( 'NONE', *, *, #3025, .T. ) ;
#19461 = CARTESIAN_POINT ( 'NONE',  ( -15.73057431336374101, -9.936106390668207666, 3.494968291668457905 ) ) ;
#19462 = DIRECTION ( 'NONE',  ( 1.000000000000000000, 0.000000000000000000, 0.000000000000000000 ) ) ;
#19463 = DIRECTION ( 'NONE',  ( -1.000000000000000000, 0.000000000000000000, 0.000000000000000000 ) ) ;
#19464 =( NAMED_UNIT ( * ) SI_UNIT ( $, .STERADIAN. ) SOLID_ANGLE_UNIT ( ) );
#19465 = EDGE_CURVE ( 'NONE', #10425, #2252, #53, .T. ) ;
#19466 = EDGE_LOOP ( 'NONE', ( #10467, #15554, #1253, #4341, #8565, #11834, #16129, #18777, #22823 ) ) ;
#19467 = LINE ( 'NONE', #18973, #4159 ) ;
#19468 = CARTESIAN_POINT ( 'NONE',  ( -4.364690642044310565, 15.35159745129469755, -4.297429366192518252 ) ) ;
#19469 = CARTESIAN_POINT ( 'NONE',  ( -22.93483120822000032, -10.59336881657999996, -3.621420100782999807 ) ) ;
#19470 = EDGE_CURVE ( 'NONE', #5466, #12394, #23030, .T. ) ;
#19471 = CARTESIAN_POINT ( 'NONE',  ( -17.05110591912999851, 10.19050343432999917, -3.717068697430999880 ) ) ;
#19472 = CARTESIAN_POINT ( 'NONE',  ( -6.218877990892996976, 16.13966241814000213, 0.9717607918608996975 ) ) ;
#19473 = EDGE_CURVE ( 'NONE', #10339, #14083, #19961, .T. ) ;
#19474 = CARTESIAN_POINT ( 'NONE',  ( 13.36494494526000132, 7.290979141362999627, -7.150624518174999444 ) ) ;
#19475 = CARTESIAN_POINT ( 'NONE',  ( 5.302302355349000074, 1.578914512950999657E-14, -14.43375672973994917 ) ) ;
#19476 =( GEOMETRIC_REPRESENTATION_CONTEXT ( 3 ) GLOBAL_UNCERTAINTY_ASSIGNED_CONTEXT ( ( #3345 ) ) GLOBAL_UNIT_ASSIGNED_CONTEXT ( ( #6500, #21398, #19464 ) ) REPRESENTATION_CONTEXT ( 'NONE', 'WORKASPACE' ) );
#19477 = DIRECTION ( 'NONE',  ( -0.7071067811865474617, 0.7071067811865474617, 0.000000000000000000 ) ) ;
#19478 = CARTESIAN_POINT ( 'NONE',  ( -1.989999999999999991, 0.000000000000000000, 0.000000000000000000 ) ) ;
#19479 = VERTEX_POINT ( 'NONE', #206 ) ;
#19480 = FACE_OUTER_BOUND ( 'NONE', #7153, .T. ) ;
#19481 = CARTESIAN_POINT ( 'NONE',  ( -1.603077936557000038, 27.73913313894999888, -1.876963106047000007 ) ) ;
#19482 = AXIS2_PLACEMENT_3D ( 'NONE', #6069, #4273, #17217 ) ;
#19483 = DIRECTION ( 'NONE',  ( 0.000000000000000000, 1.000000000000000000, 0.000000000000000000 ) ) ;
#19484 = B_SPLINE_CURVE_WITH_KNOTS ( 'NONE', 3,
 ( #16766, #294, #20774, #14945 ),
 .UNSPECIFIED., .F., .F.,
 ( 4, 4 ),
 ( 0.000000000000000000, 1.000000000000000000 ),
 .UNSPECIFIED. ) ;
#19485 = CARTESIAN_POINT ( 'NONE',  ( -14.50687460260128425, 1.490768935493058889, -8.918514818220842244 ) ) ;
#19486 = CARTESIAN_POINT ( 'NONE',  ( 2.411379030285999647, 28.19187716036000069, 0.4306175354954999701 ) ) ;
#19487 = EDGE_CURVE ( 'NONE', #18434, #8639, #1390, .T. ) ;
#19488 = EDGE_CURVE ( 'NONE', #23321, #2821, #10508, .T. ) ;
#19489 = LINE ( 'NONE', #19367, #8086 ) ;
#19490 = VERTEX_POINT ( 'NONE', #2269 ) ;
#19491 = DIRECTION ( 'NONE',  ( 1.000000000000000000, 0.000000000000000000, 0.000000000000000000 ) ) ;
#19492 = CARTESIAN_POINT ( 'NONE',  ( 3.928282035707792552, 12.12595830749078374, -2.822092405151465755 ) ) ;
#19493 = DIRECTION ( 'NONE',  ( 1.000000000000000000, 0.000000000000000000, 0.000000000000000000 ) ) ;
#19494 = CARTESIAN_POINT ( 'NONE',  ( -0.5912276634582656065, 6.803124766514241806, 1.648605811313639702 ) ) ;
#19495 = FACE_OUTER_BOUND ( 'NONE', #15825, .T. ) ;
#19496 = CARTESIAN_POINT ( 'NONE',  ( -11.82164471169000208, -0.5931465403154000393, 15.55754198224000007 ) ) ;
#19497 = CARTESIAN_POINT ( 'NONE',  ( -13.44269301469999967, -0.9911996677733001526, -11.23901760903999936 ) ) ;
#19498 = CARTESIAN_POINT ( 'NONE',  ( 15.99918875730999979, 7.956028365285000348, 4.607548929765999723 ) ) ;
#19499 = CARTESIAN_POINT ( 'NONE',  ( 18.93524367559212607, 2.269347932775633403, 10.18482703568339787 ) ) ;
#19500 = VERTEX_POINT ( 'NONE', #11844 ) ;
#19501 = DIRECTION ( 'NONE',  ( -0.5000000000000169864, 0.8660254037844288266, 0.000000000000000000 ) ) ;
#19502 = CARTESIAN_POINT ( 'NONE',  ( 2.330854569989000424, 30.66143933041000125, -0.2259880098311999874 ) ) ;
#19503 = CARTESIAN_POINT ( 'NONE',  ( -11.00000000000000000, -7.200000000000000178, 0.000000000000000000 ) ) ;
#19504 = CARTESIAN_POINT ( 'NONE',  ( 0.2037756909558023355, 13.66463196969724869, -6.169302963772167026 ) ) ;
#19505 = B_SPLINE_CURVE_WITH_KNOTS ( 'NONE', 3,
 ( #17233, #636, #20637, #8036, #2108, #162, #4048, #7552, #5623, #20407 ),
 .UNSPECIFIED., .F., .F.,
 ( 4, 2, 2, 2, 4 ),
 ( 0.000000000000000000, 0.2500000000000000000, 0.5000000000000000000, 0.7500000000000000000, 1.000000000000000000 ),
 .UNSPECIFIED. ) ;
#19506 = ORIENTED_EDGE ( 'NONE', *, *, #10987, .T. ) ;
#19507 = CYLINDRICAL_SURFACE ( 'NONE', #12575, 4.750000000000000000 ) ;
#19508 = DIRECTION ( 'NONE',  ( 0.000000000000000000, 0.000000000000000000, -1.000000000000000000 ) ) ;
#19509 = DIRECTION ( 'NONE',  ( -1.000000000000000000, 0.000000000000000000, 0.000000000000000000 ) ) ;
#19510 = CARTESIAN_POINT ( 'NONE',  ( 0.000000000000000000, 26.50000000000000355, 0.000000000000000000 ) ) ;
#19511 = CARTESIAN_POINT ( 'NONE',  ( 14.22488390888686105, -1.430681673238417106, -10.26079249266155280 ) ) ;
#19512 = DIRECTION ( 'NONE',  ( 1.000000000000000000, 0.000000000000000000, 0.000000000000000000 ) ) ;
#19513 = DIRECTION ( 'NONE',  ( 0.000000000000000000, -1.000000000000000000, 0.000000000000000000 ) ) ;
#19514 = AXIS2_PLACEMENT_3D ( 'NONE', #136, #15029, #14908 ) ;
#19515 = DIRECTION ( 'NONE',  ( 0.000000000000000000, 1.000000000000000000, 0.000000000000000000 ) ) ;
#19516 = ORIENTED_EDGE ( 'NONE', *, *, #20897, .F. ) ;
#19517 = CARTESIAN_POINT ( 'NONE',  ( -24.50000000000000000, -8.081477262649000792, -6.807253044743999837 ) ) ;
#19518 = CARTESIAN_POINT ( 'NONE',  ( 12.52688711657000020, -7.716878364870000340, 11.63397459621999985 ) ) ;
#19519 = ORIENTED_EDGE ( 'NONE', *, *, #18855, .F. ) ;
#19520 = CARTESIAN_POINT ( 'NONE',  ( 1.815435739943000115, 24.25568479955999734, 1.783857804741999953 ) ) ;
#19521 = CARTESIAN_POINT ( 'NONE',  ( -1.376955291490763233, 24.71727056350960794, 1.708239419793794456 ) ) ;
#19522 = CARTESIAN_POINT ( 'NONE',  ( 3.577690694476612254, 13.23335103741512775, 5.763370895648841419 ) ) ;
#19523 = AXIS2_PLACEMENT_3D ( 'NONE', #11712, #431, #7832 ) ;
#19524 = CARTESIAN_POINT ( 'NONE',  ( 6.152345744605784539, 14.11688686930400927, -0.2931242286481389181 ) ) ;
#19525 = CARTESIAN_POINT ( 'NONE',  ( -20.88996149064833929, 7.734893377964897176, 5.108810731787540860 ) ) ;
#19526 = DIRECTION ( 'NONE',  ( 0.9996708941621507138, 0.02565352539215873945, 0.000000000000000000 ) ) ;
#19527 = ORIENTED_EDGE ( 'NONE', *, *, #16950, .T. ) ;
#19528 = CARTESIAN_POINT ( 'NONE',  ( -8.035714285714000482, 9.574826156038998448, 0.000000000000000000 ) ) ;
#19529 = CIRCLE ( 'NONE', #1357, 13.93375672974000068 ) ;
#19530 = CARTESIAN_POINT ( 'NONE',  ( 3.824747490998164245, 24.75094615491877548, 2.410583160007404580 ) ) ;
#19531 = CARTESIAN_POINT ( 'NONE',  ( -19.10482910584000038, 1.458613477275000161E-14, 0.000000000000000000 ) ) ;
#19532 = ORIENTED_EDGE ( 'NONE', *, *, #13562, .T. ) ;
#19533 = CARTESIAN_POINT ( 'NONE',  ( -20.01793400091000308, 5.566461610995999898, -8.487890939669000545 ) ) ;
#19534 = CARTESIAN_POINT ( 'NONE',  ( 3.316314694148171593, 28.12756664670257933, -2.704122461039529579 ) ) ;
#19535 = CARTESIAN_POINT ( 'NONE',  ( 2.000000000000000000, 18.27087121525220681, 1.096451616434099242E-10 ) ) ;
#19536 = CARTESIAN_POINT ( 'NONE',  ( 14.95177042847206117, 10.28604982897092235, 1.247623827059667345 ) ) ;
#19537 = STYLED_ITEM ( 'NONE', ( #9111 ), #9053 ) ;
#19538 = FACE_OUTER_BOUND ( 'NONE', #20357, .T. ) ;
#19539 = FACE_OUTER_BOUND ( 'NONE', #2400, .T. ) ;
#19540 = CARTESIAN_POINT ( 'NONE',  ( -22.33796067008437447, -9.002300166801388670, 2.420455048598586512 ) ) ;
#19541 = CARTESIAN_POINT ( 'NONE',  ( -4.341996183777002472, 12.31336825867998641, -2.011830581554000297 ) ) ;
#19542 = ORIENTED_EDGE ( 'NONE', *, *, #14392, .F. ) ;
#19543 = CARTESIAN_POINT ( 'NONE',  ( -13.23956266673000037, 6.512279107760999608, -9.204720484723999618 ) ) ;
#19544 = CARTESIAN_POINT ( 'NONE',  ( -2.071691020321107857, 29.44040781721670186, 0.6104882387633735474 ) ) ;
#19545 = ORIENTED_EDGE ( 'NONE', *, *, #6527, .T. ) ;
#19546 = CARTESIAN_POINT ( 'NONE',  ( -7.590990257669999686, 26.59099025766972701, -6.000000000000000000 ) ) ;
#19547 = CIRCLE ( 'NONE', #9096, 4.750000000000000000 ) ;
#19548 = CARTESIAN_POINT ( 'NONE',  ( -14.40513632270981681, -2.351574831385553566, 10.08995167311471874 ) ) ;
#19549 = ORIENTED_EDGE ( 'NONE', *, *, #12449, .T. ) ;
#19550 = DIRECTION ( 'NONE',  ( 0.000000000000000000, 0.000000000000000000, -1.000000000000000000 ) ) ;
#19551 = CARTESIAN_POINT ( 'NONE',  ( 5.749772404096996858, 14.16353669839999441, -1.990178937412000471 ) ) ;
#19552 = CARTESIAN_POINT ( 'NONE',  ( 1.835060406389813270, 27.99999999999983658, 3.559329533908949461 ) ) ;
#19553 = CARTESIAN_POINT ( 'NONE',  ( -8.000000000000000000, 1.322618543078999814E-14, 0.000000000000000000 ) ) ;
#19554 = EDGE_CURVE ( 'NONE', #8792, #19900, #9663, .T. ) ;
#19555 = CARTESIAN_POINT ( 'NONE',  ( 12.65175158531000044, 9.909822556590000886, -2.072115565883000166 ) ) ;
#19556 = ORIENTED_EDGE ( 'NONE', *, *, #13487, .F. ) ;
#19557 = CARTESIAN_POINT ( 'NONE',  ( 0.000000000000000000, 24.50000000000000000, 0.000000000000000000 ) ) ;
#19558 = CARTESIAN_POINT ( 'NONE',  ( -2.500000000000000444, 27.18333333333333357, -0.3272492347489320275 ) ) ;
#19559 = DIRECTION ( 'NONE',  ( -1.000000000000000000, 0.000000000000000000, 0.000000000000000000 ) ) ;
#19560 = ORIENTED_EDGE ( 'NONE', *, *, #19584, .F. ) ;
#19561 = DIRECTION ( 'NONE',  ( 0.000000000000000000, 1.000000000000000000, 0.000000000000000000 ) ) ;
#19562 = CARTESIAN_POINT ( 'NONE',  ( 11.55284350195684340, 12.59061462091154837, 3.192208964413439709 ) ) ;
#19563 = CARTESIAN_POINT ( 'NONE',  ( -23.50032910583999879, 3.801543240379000377, -8.459419100777001432 ) ) ;
#19564 = AXIS2_PLACEMENT_3D ( 'NONE', #22846, #17163, #20683 ) ;
#19565 = CARTESIAN_POINT ( 'NONE',  ( -5.091020417477109206, 13.90168003929542273, -5.423969081848736273 ) ) ;
#19566 = CARTESIAN_POINT ( 'NONE',  ( 16.49585459645880192, 7.156609457148421782, -7.549996209224957511 ) ) ;
#19567 = CARTESIAN_POINT ( 'NONE',  ( 23.99062354302999722, -7.716878364870000340, -11.63397459621999985 ) ) ;
#19568 = EDGE_CURVE ( 'NONE', #14405, #7738, #18028, .T. ) ;
#19569 = CARTESIAN_POINT ( 'NONE',  ( -14.47826291725376358, 11.73192043637804893, -4.679722760534376746 ) ) ;
#19570 = CARTESIAN_POINT ( 'NONE',  ( -3.826948838359951477, 14.04946500315414148, -4.851233642384933376 ) ) ;
#19571 = CARTESIAN_POINT ( 'NONE',  ( -1.722646045537596704, 30.12122296660216847, -1.303888318235613353 ) ) ;
#19572 = ORIENTED_EDGE ( 'NONE', *, *, #17881, .T. ) ;
#19573 = CARTESIAN_POINT ( 'NONE',  ( -24.36724102301948847, -2.559142463821917346, 12.49991998441870145 ) ) ;
#19574 = CARTESIAN_POINT ( 'NONE',  ( 19.89308446879999792, 10.49337901864999978, -2.757826031130999667 ) ) ;
#19575 = CARTESIAN_POINT ( 'NONE',  ( 24.38501637916864340, 2.018571612540227544, 10.43313927157142729 ) ) ;
#19576 = LINE ( 'NONE', #14115, #7208 ) ;
#19577 = ORIENTED_EDGE ( 'NONE', *, *, #20092, .F. ) ;
#19578 = CARTESIAN_POINT ( 'NONE',  ( -20.43006341542451310, 6.446850357970787648, -8.297382802253483902 ) ) ;
#19579 = VECTOR ( 'NONE', #37, 1000.000000000000114 ) ;
#19580 = CARTESIAN_POINT ( 'NONE',  ( -24.46742986865170622, -11.46616815103349118, -5.140026613645124698 ) ) ;
#19581 = VECTOR ( 'NONE', #20025, 1000.000000000000000 ) ;
#19582 = CARTESIAN_POINT ( 'NONE',  ( -2.805898255323001411, 11.85722042793000952, -4.087626962984003853 ) ) ;
#19583 = ORIENTED_EDGE ( 'NONE', *, *, #12798, .F. ) ;
#19584 = EDGE_CURVE ( 'NONE', #11532, #13012, #18761, .T. ) ;
#19585 = CARTESIAN_POINT ( 'NONE',  ( -16.54000019300971402, 10.40780738326815680, -0.02728000515637632115 ) ) ;
#19586 = CARTESIAN_POINT ( 'NONE',  ( -4.000000000000073719, 24.70197603011089527, -1.905018119001588683 ) ) ;
#19587 = CARTESIAN_POINT ( 'NONE',  ( 0.5551539414043799026, 26.26248452079970619, 2.089084675604010233 ) ) ;
#19588 = CARTESIAN_POINT ( 'NONE',  ( -14.43045987140080300, -3.231330187232687834, -12.49999333233078325 ) ) ;
#19589 = ORIENTED_EDGE ( 'NONE', *, *, #896, .F. ) ;
#19590 = CARTESIAN_POINT ( 'NONE',  ( -1.767805011140364924, 26.50018596745192312, 1.767686163102024643 ) ) ;
#19591 = CARTESIAN_POINT ( 'NONE',  ( -12.09893706263999924, 13.67685060524999940, -6.159850446377999056 ) ) ;
#19592 = CARTESIAN_POINT ( 'NONE',  ( -21.97131109840999841, 9.664045591200999041, 5.599833161489999434 ) ) ;
#19593 = ADVANCED_FACE ( 'NONE', ( #17043 ), #16921, .F. ) ;
#19594 = CARTESIAN_POINT ( 'NONE',  ( -17.52341705246000103, 5.107418338671999791, -8.973179355929001844 ) ) ;
#19595 = CARTESIAN_POINT ( 'NONE',  ( 22.04058333333331987, -8.996523669780138732, -2.417618220618300562 ) ) ;
#19596 = CARTESIAN_POINT ( 'NONE',  ( 17.22431994525999954, 10.31730248877000022, 0.2667559614094999754 ) ) ;
#19597 = FACE_OUTER_BOUND ( 'NONE', #21366, .T. ) ;
#19598 = CIRCLE ( 'NONE', #19993, 1.000000000000000666 ) ;
#19599 = AXIS2_PLACEMENT_3D ( 'NONE', #23484, #15721, #12476 ) ;
#19600 = CARTESIAN_POINT ( 'NONE',  ( 19.87622032598000033, -3.917852614669999234, 8.831257209013999798 ) ) ;
#19601 = CARTESIAN_POINT ( 'NONE',  ( 15.35145833333333165, 5.570917836446059646, -7.249253927134781783 ) ) ;
#19602 = EDGE_LOOP ( 'NONE', ( #10306, #3172, #14479 ) ) ;
#19603 = CARTESIAN_POINT ( 'NONE',  ( 2.263570575011602859, 13.94136812588888041, 5.692591906759779441 ) ) ;
#19604 = CARTESIAN_POINT ( 'NONE',  ( 1.403495832404999977, 26.65869850838000232, -1.780325977227999790 ) ) ;
#19605 = ADVANCED_FACE ( 'NONE', ( #5899 ), #4871, .F. ) ;
#19606 = CARTESIAN_POINT ( 'NONE',  ( -19.50887077250665413, 5.636661757442777976, -7.334388769936609265 ) ) ;
#19607 = CARTESIAN_POINT ( 'NONE',  ( -14.24706062280937502, 7.999159735059844678, -4.368120482967156271 ) ) ;
#19608 = CARTESIAN_POINT ( 'NONE',  ( 1.732076717456000114, 27.31437716035999941, 1.732076717456000114 ) ) ;
#19609 = CARTESIAN_POINT ( 'NONE',  ( -4.744723115955535420, 12.41001117572974088, 0.9970819178471495015 ) ) ;
#19610 = ORIENTED_EDGE ( 'NONE', *, *, #18134, .F. ) ;
#19611 = ADVANCED_FACE ( 'NONE', ( #15212 ), #687, .T. ) ;
#19612 = CARTESIAN_POINT ( 'NONE',  ( 4.724609123937420385, 12.40245730446895323, -1.087195817531082076 ) ) ;
#19613 = CARTESIAN_POINT ( 'NONE',  ( -3.963044985152003097, 14.56862624118001825, 4.679621608874002803 ) ) ;
#19614 = EDGE_CURVE ( 'NONE', #17324, #20493, #11432, .T. ) ;
#19615 = CIRCLE ( 'NONE', #7612, 4.000000000000000000 ) ;
#19616 = CARTESIAN_POINT ( 'NONE',  ( 11.49246134983401113, -8.135562067959659416, -3.829935661804423130 ) ) ;
#19617 = DIRECTION ( 'NONE',  ( -5.702245064659998234E-10, 0.9999999999999997780, 2.283934677740999354E-08 ) ) ;
#19618 = CARTESIAN_POINT ( 'NONE',  ( -2.213186668863544426, 30.78310712015282036, -0.2500141473247705082 ) ) ;
#19619 = CARTESIAN_POINT ( 'NONE',  ( -6.115711741633154119, 15.99577490368180044, -1.049722815977955026 ) ) ;
#19620 = CARTESIAN_POINT ( 'NONE',  ( 14.81906392131000061, -2.842327771818999871, 9.244929856806999524 ) ) ;
#19621 = CARTESIAN_POINT ( 'NONE',  ( 24.50000000000000000, 10.82531754731000007, -6.250000000000000000 ) ) ;
#19622 = ORIENTED_EDGE ( 'NONE', *, *, #11891, .F. ) ;
#19623 = ADVANCED_FACE ( 'NONE', ( #4092 ), #9502, .F. ) ;
#19624 = CARTESIAN_POINT ( 'NONE',  ( -22.34263658169068378, -2.418798806450678907, 9.002255236133725802 ) ) ;
#19625 = CARTESIAN_POINT ( 'NONE',  ( 1.795439626675999989, 29.15163585920999978, 2.048365916996000458 ) ) ;
#19626 = CARTESIAN_POINT ( 'NONE',  ( -15.23841243917333266, 2.371928265978177741, 8.826509812641717190 ) ) ;
#19627 = CARTESIAN_POINT ( 'NONE',  ( -6.250000000000000000, 16.31160201366999729, -2.000000000000000000 ) ) ;
#19628 = EDGE_LOOP ( 'NONE', ( #22802, #8963, #17668, #21109, #1345, #3384 ) ) ;
#19629 = CIRCLE ( 'NONE', #22302, 2.399999999999999911 ) ;
#19630 = CARTESIAN_POINT ( 'NONE',  ( -5.833999999999999631, 1.198997689148999791E-14, -12.89775331292463711 ) ) ;
#19631 = CARTESIAN_POINT ( 'NONE',  ( -24.50000000000293099, 11.08154813084197698, -5.806195610872452839 ) ) ;
#19632 = CARTESIAN_POINT ( 'NONE',  ( 4.000000000000000000, 24.80000000000000426, -2.309401076759000304 ) ) ;
#19633 = CARTESIAN_POINT ( 'NONE',  ( -12.50000000000000000, 6.606768802097000126, -6.099810110451000966 ) ) ;
#19634 = CIRCLE ( 'NONE', #15347, 2.999999999999999112 ) ;
#19635 = CARTESIAN_POINT ( 'NONE',  ( -4.239658300008966485, 13.64990765111504167, 4.928031708687682588 ) ) ;
#19636 = CARTESIAN_POINT ( 'NONE',  ( 0.000000000000000000, 18.50000000000000000, 0.000000000000000000 ) ) ;
#19637 = CARTESIAN_POINT ( 'NONE',  ( 20.01958103379666198, -1.202189832516999735, 9.185023618884988750 ) ) ;
#19638 = ORIENTED_EDGE ( 'NONE', *, *, #6133, .T. ) ;
#19639 = CARTESIAN_POINT ( 'NONE',  ( -0.9538268690393967297, 30.53169873023693626, 2.326930193732148044 ) ) ;
#19640 = DIRECTION ( 'NONE',  ( 0.000000000000000000, 1.000000000000000000, 0.000000000000000000 ) ) ;
#19641 = ORIENTED_EDGE ( 'NONE', *, *, #17364, .F. ) ;
#19642 = ADVANCED_FACE ( 'NONE', ( #2508 ), #13643, .T. ) ;
#19643 = CARTESIAN_POINT ( 'NONE',  ( 5.639929954731005779, 14.19535997545999351, 2.283685262506000235 ) ) ;
#19644 = DIRECTION ( 'NONE',  ( -1.000000000000000000, 0.000000000000000000, 0.000000000000000000 ) ) ;
#19645 = EDGE_CURVE ( 'NONE', #21756, #15884, #20703, .T. ) ;
#19646 = CIRCLE ( 'NONE', #266, 4.549999999999999822 ) ;
#19647 = CARTESIAN_POINT ( 'NONE',  ( 6.232362344166777035, 13.72735485794549426, -1.446143930354119922 ) ) ;
#19648 = DIRECTION ( 'NONE',  ( -1.000000000000000000, 0.000000000000000000, 0.000000000000000000 ) ) ;
#19649 = ORIENTED_EDGE ( 'NONE', *, *, #6404, .F. ) ;
#19650 = CARTESIAN_POINT ( 'NONE',  ( 2.500000000000000000, 30.23419673619000037, 0.000000000000000000 ) ) ;
#19651 = CARTESIAN_POINT ( 'NONE',  ( 0.2258413948657297943, 26.24995681965566519, 2.153052638588166978 ) ) ;
#19652 = CARTESIAN_POINT ( 'NONE',  ( -20.21721940389334193, -9.008888981094067105, 2.097083988089771811 ) ) ;
#19653 = ORIENTED_EDGE ( 'NONE', *, *, #17646, .T. ) ;
#19654 = EDGE_CURVE ( 'NONE', #44, #7629, #5250, .T. ) ;
#19655 = CARTESIAN_POINT ( 'NONE',  ( -24.73275700429000068, -10.85635561503000091, -0.8019128780756998864 ) ) ;
#19656 = EDGE_CURVE ( 'NONE', #2037, #8899, #15659, .T. ) ;
#19657 = CARTESIAN_POINT ( 'NONE',  ( 20.75566666666665583, 4.635148009726169249, -8.042302503330198249 ) ) ;
#19658 = CARTESIAN_POINT ( 'NONE',  ( 15.06172671233659699, 9.055098203261204404, 4.981601320280216960 ) ) ;
#19659 = DIRECTION ( 'NONE',  ( 1.000000000000000000, 0.000000000000000000, 0.000000000000000000 ) ) ;
#19660 = CARTESIAN_POINT ( 'NONE',  ( 1.181632374602280988, 24.55137445130629104, 3.936586548167761990 ) ) ;
#19661 = CARTESIAN_POINT ( 'NONE',  ( -22.98076624016430713, 7.404256252206974587, 5.690969114276820839 ) ) ;
#19662 = CARTESIAN_POINT ( 'NONE',  ( -1.402221074164999637, 11.71985185161000587, -4.549932804316000556 ) ) ;
#19663 = ORIENTED_EDGE ( 'NONE', *, *, #3608, .T. ) ;
#19664 = AXIS2_PLACEMENT_3D ( 'NONE', #13516, #6367, #11829 ) ;
#19665 = B_SPLINE_CURVE_WITH_KNOTS ( 'NONE', 3,
 ( #534, #5877, #15305, #22819, #4182, #18835, #9635, #9872, #7700, #22585 ),
 .UNSPECIFIED., .F., .F.,
 ( 4, 1, 1, 2, 2, 4 ),
 ( 0.000000000000000000, 0.2499999999999969469, 0.3749999999999960032, 0.4374999999999962252, 0.4999999999999963363, 1.000000000000000000 ),
 .UNSPECIFIED. ) ;
#19666 = CARTESIAN_POINT ( 'NONE',  ( -24.43680486115877670, -9.658061704670100056, -3.574636863997652902 ) ) ;
#19667 = CARTESIAN_POINT ( 'NONE',  ( -2.071136996602504610, 29.44052298352770691, 0.6123601400604211653 ) ) ;
#19668 = EDGE_LOOP ( 'NONE', ( #21112, #1470, #16077, #15897 ) ) ;
#19669 = CARTESIAN_POINT ( 'NONE',  ( -6.046835300290999804, 16.30334124114000360, 1.000000020649999932 ) ) ;
#19670 = CARTESIAN_POINT ( 'NONE',  ( -17.41481040294117122, -7.305510571727924507, -7.454128842472707461 ) ) ;
#19671 = ORIENTED_EDGE ( 'NONE', *, *, #18565, .F. ) ;
#19672 = AXIS2_PLACEMENT_3D ( 'NONE', #10547, #12482, #14830 ) ;
#19673 = CARTESIAN_POINT ( 'NONE',  ( -7.500000000000000000, 18.50000000000000000, -5.000000000000000000 ) ) ;
#19674 = CARTESIAN_POINT ( 'NONE',  ( 5.383802162386005286, 13.84993582567999582, -3.902720988293997717 ) ) ;
#19675 = CARTESIAN_POINT ( 'NONE',  ( 12.00000000000000355, -2.741782068716092535, -8.563895310330577715 ) ) ;
#19676 = CARTESIAN_POINT ( 'NONE',  ( 17.54649695406000021, -10.67134204638000128, -3.051581116462999788 ) ) ;
#19677 = CARTESIAN_POINT ( 'NONE',  ( 14.40675158531000122, 9.325397517960999139, -4.058504152148000088 ) ) ;
#19678 = ORIENTED_EDGE ( 'NONE', *, *, #4145, .F. ) ;
#19679 = DIRECTION ( 'NONE',  ( 1.000000000000000000, 0.000000000000000000, 0.000000000000000000 ) ) ;
#19680 = AXIS2_PLACEMENT_3D ( 'NONE', #3661, #23529, #14444 ) ;
#19681 = CARTESIAN_POINT ( 'NONE',  ( 0.000000000000000000, 14.43375672974000068, 0.000000000000000000 ) ) ;
#19682 = EDGE_LOOP ( 'NONE', ( #2977, #20789, #7232, #22736 ) ) ;
#19683 = FACE_OUTER_BOUND ( 'NONE', #1317, .T. ) ;
#19684 = CARTESIAN_POINT ( 'NONE',  ( 24.47069144955800368, -7.568636691949420126, 7.463144728829862018 ) ) ;
#19685 = CARTESIAN_POINT ( 'NONE',  ( -13.99999999999999645, 3.409677747946862070, 8.987483889666412651 ) ) ;
#19686 = CARTESIAN_POINT ( 'NONE',  ( 17.28855324646004021, -3.723961278307348799, 9.741530358186297534 ) ) ;
#19687 = CARTESIAN_POINT ( 'NONE',  ( -19.05537077250666300, 7.325082484084620482, 5.629509844743244784 ) ) ;
#19688 = AXIS2_PLACEMENT_3D ( 'NONE', #4363, #22525, #7878 ) ;
#19689 = CARTESIAN_POINT ( 'NONE',  ( -14.49454819745152356, 10.30763366379271062, -7.146668779517979964 ) ) ;
#19690 = CIRCLE ( 'NONE', #12343, 5.000000000000004441 ) ;
#19691 = CONICAL_SURFACE ( 'NONE', #10791, 9.136555860486998526, 0.02565634000431304615 ) ;
#19692 = CARTESIAN_POINT ( 'NONE',  ( -4.218945794843817154, 13.66537927080853976, -4.919477749078775553 ) ) ;
#19693 = CARTESIAN_POINT ( 'NONE',  ( -1.270048396745602881, 30.32394092141509745, 1.751222398791842050 ) ) ;
#19694 = VERTEX_POINT ( 'NONE', #19223 ) ;
#19695 = CARTESIAN_POINT ( 'NONE',  ( -1.727993674177999983, 25.50834080394000125, 1.571450918520000073 ) ) ;
#19696 = CARTESIAN_POINT ( 'NONE',  ( 21.82559380440000396, 10.77499779627999921, 1.666852620760000070 ) ) ;
#19697 = CARTESIAN_POINT ( 'NONE',  ( 23.76080193858683742, 7.519392389711364366, -7.487444224767115131 ) ) ;
#19698 = CARTESIAN_POINT ( 'NONE',  ( 12.00000000000000000, 10.65000000000000036, 0.000000000000000000 ) ) ;
#19699 = VECTOR ( 'NONE', #21485, 1000.000000000000000 ) ;
#19700 = ORIENTED_EDGE ( 'NONE', *, *, #9489, .T. ) ;
#19701 = CYLINDRICAL_SURFACE ( 'NONE', #5279, 3.000000000000000000 ) ;
#19702 = CARTESIAN_POINT ( 'NONE',  ( 4.852944915824914496, 14.55942026833422354, 3.781726298951809451 ) ) ;
#19703 = B_SPLINE_CURVE_WITH_KNOTS ( 'NONE', 3,
 ( #1660, #7822, #9167, #12910, #22348, #9518, #15192, #9403, #2129, #14836, #20780, #18487, #5641, #7705, #13152, #20659, #13027, #11232 ),
 .UNSPECIFIED., .F., .F.,
 ( 4, 2, 2, 2, 2, 2, 2, 2, 4 ),
 ( 0.000000000000000000, 0.1249999999999999722, 0.2500000000000000000, 0.3750000000000000000, 0.5000000000000001110, 0.6250000000000001110, 0.7500000000000000000, 0.8750000000000000000, 1.000000000000000000 ),
 .UNSPECIFIED. ) ;
#19704 = DIRECTION ( 'NONE',  ( -1.000000000000000000, 0.000000000000000000, 0.000000000000000000 ) ) ;
#19705 = ORIENTED_EDGE ( 'NONE', *, *, #2464, .F. ) ;
#19706 = AXIS2_PLACEMENT_3D ( 'NONE', #1094, #15735, #12005 ) ;
#19707 = CARTESIAN_POINT ( 'NONE',  ( -15.20026080601097540, -0.7701753238851960504, -10.34310266448994042 ) ) ;
#19708 = LINE ( 'NONE', #21757, #20041 ) ;
#19709 = EDGE_LOOP ( 'NONE', ( #4532, #3138, #6053, #14163 ) ) ;
#19710 = VECTOR ( 'NONE', #17040, 1000.000000000000000 ) ;
#19711 = CARTESIAN_POINT ( 'NONE',  ( 3.000000000000000000, 17.00000000000000000, 0.000000000000000000 ) ) ;
#19712 =( NAMED_UNIT ( * ) PLANE_ANGLE_UNIT ( ) SI_UNIT ( $, .RADIAN. ) );
#19713 = DIRECTION ( 'NONE',  ( -1.000000000000000000, 0.000000000000000000, 0.000000000000000000 ) ) ;
#19714 = ORIENTED_EDGE ( 'NONE', *, *, #19027, .T. ) ;
#19715 = DIRECTION ( 'NONE',  ( 0.000000000000000000, 0.000000000000000000, 1.000000000000000000 ) ) ;
#19716 = CIRCLE ( 'NONE', #8492, 3.050000000000000266 ) ;
#19717 = CARTESIAN_POINT ( 'NONE',  ( -12.23285353330000014, 13.67685060524999940, -6.159850446377999056 ) ) ;
#19718 = CARTESIAN_POINT ( 'NONE',  ( -24.86648035909999876, 8.837410641880000028, -3.973955761889000016 ) ) ;
#19719 = CARTESIAN_POINT ( 'NONE',  ( -18.67614870288999995, 10.39069081642000114, 3.268177410067999666 ) ) ;
#19720 = CARTESIAN_POINT ( 'NONE',  ( -6.314291400897996454, 15.85600325500998942, 1.061606865039998571 ) ) ;
#19721 = CARTESIAN_POINT ( 'NONE',  ( 17.83369494525999954, -5.541591344052999801, 8.726939668821000140 ) ) ;
#19722 = CARTESIAN_POINT ( 'NONE',  ( -14.25699038479000080, -13.93375672974000068, -0.1440397836109000018 ) ) ;
#19723 = CARTESIAN_POINT ( 'NONE',  ( 20.93851493891000004, 7.913501176053999053, -5.593456792387000220 ) ) ;
#19724 = CIRCLE ( 'NONE', #8114, 10.65000000000000036 ) ;
#19725 = EDGE_CURVE ( 'NONE', #18459, #8533, #8999, .T. ) ;
#19726 = CARTESIAN_POINT ( 'NONE',  ( 24.37713355803436599, -9.330746210554012876, 8.838673490789293652 ) ) ;
#19727 = ORIENTED_EDGE ( 'NONE', *, *, #8923, .T. ) ;
#19728 = CARTESIAN_POINT ( 'NONE',  ( 23.50918822630940141, 3.211384162367111550, 8.722405065347860642 ) ) ;
#19729 = CARTESIAN_POINT ( 'NONE',  ( -1.736679406361667288, 13.83192101583320444, 5.887765559668492799 ) ) ;
#19730 = CARTESIAN_POINT ( 'NONE',  ( -0.6232602838478999985, 26.08163313895000002, -2.388357610153000188 ) ) ;
#19731 = AXIS2_PLACEMENT_3D ( 'NONE', #19358, #10394, #10149 ) ;
#19732 = VECTOR ( 'NONE', #18633, 1000.000000000000000 ) ;
#19733 = CARTESIAN_POINT ( 'NONE',  ( -20.07574577250665016, -8.947317243346674331, -2.404655041047230934 ) ) ;
#19734 = CARTESIAN_POINT ( 'NONE',  ( -19.74309982448999889, -9.328357949534000326, 5.911015106955000320 ) ) ;
#19735 = CARTESIAN_POINT ( 'NONE',  ( -4.000693775878768399, 12.14919889384218443, 2.720895155930553866 ) ) ;
#19736 = EDGE_LOOP ( 'NONE', ( #17587, #16042 ) ) ;
#19737 = CARTESIAN_POINT ( 'NONE',  ( 0.000000000000000000, 29.69999999999999929, -2.100000000000000089 ) ) ;
#19738 = CARTESIAN_POINT ( 'NONE',  ( 4.469428354791611824, 12.30899859160570031, -1.869002996406054384 ) ) ;
#19739 = ADVANCED_FACE ( 'NONE', ( #241 ), #18773, .F. ) ;
#19740 = CARTESIAN_POINT ( 'NONE',  ( 3.316026328257057010, 28.13336607546882817, 2.704152903937933061 ) ) ;
#19741 = CARTESIAN_POINT ( 'NONE',  ( 1.750000000000001110, 7.000000000000000000, 0.1998543250812850336 ) ) ;
#19742 = DIRECTION ( 'NONE',  ( 0.000000000000000000, -1.000000000000000000, 0.000000000000000000 ) ) ;
#19743 = CARTESIAN_POINT ( 'NONE',  ( -14.66147510250999808, 10.41001213865000175, 4.437054729469999792 ) ) ;
#19744 = CARTESIAN_POINT ( 'NONE',  ( 18.21937642130999890, 4.597142045420999246, 8.611084490720001483 ) ) ;
#19745 = CARTESIAN_POINT ( 'NONE',  ( 18.80775289361148239, 6.404165465825992776, 8.237156442842801241 ) ) ;
#19746 = ORIENTED_EDGE ( 'NONE', *, *, #5047, .F. ) ;
#19747 = CARTESIAN_POINT ( 'NONE',  ( 6.696152422707000618, 26.50000000000000000, 6.000000000000000000 ) ) ;
#19748 = CARTESIAN_POINT ( 'NONE',  ( -1.377056188230000089, 31.03159284288000208, -1.991595807317999789 ) ) ;
#19749 = CARTESIAN_POINT ( 'NONE',  ( -0.3780989064092999952, 23.55641193502999897, 2.689602506303999885 ) ) ;
#19750 = CARTESIAN_POINT ( 'NONE',  ( -2.447170124667294555, 13.98365479988347282, -5.615010659020613026 ) ) ;
#19751 = AXIS2_PLACEMENT_3D ( 'NONE', #21531, #4947, #22964 ) ;
#19752 = VERTEX_POINT ( 'NONE', #593 ) ;
#19753 = CARTESIAN_POINT ( 'NONE',  ( 0.000000000000000000, 24.40000007355299871, -4.649999926447000220 ) ) ;
#19754 = CARTESIAN_POINT ( 'NONE',  ( -24.48376588670971543, 11.33649700730286192, -5.364757780030492640 ) ) ;
#19755 = EDGE_CURVE ( 'NONE', #1014, #14850, #12215, .T. ) ;
#19756 = CARTESIAN_POINT ( 'NONE',  ( 15.65379166666666677, 9.072988859205175061, 1.187524516768785787 ) ) ;
#19757 = FACE_OUTER_BOUND ( 'NONE', #274, .T. ) ;
#19758 = CARTESIAN_POINT ( 'NONE',  ( 15.56298940832826894, -10.15326298562161789, 2.230701886652393551 ) ) ;
#19759 = CARTESIAN_POINT ( 'NONE',  ( -5.730762473771000565, 28.00000000000000000, 1.577381738259000077 ) ) ;
#19760 = CARTESIAN_POINT ( 'NONE',  ( -4.944239625353997525, 12.51416432517001809, 0.1304284014165000838 ) ) ;
#19761 = DIRECTION ( 'NONE',  ( -0.9865822012466877178, 0.000000000000000000, 0.1632653061223979518 ) ) ;
#19762 = ORIENTED_EDGE ( 'NONE', *, *, #2254, .F. ) ;
#19763 = CARTESIAN_POINT ( 'NONE',  ( 0.4901246258882320794, 30.57924682558974538, 2.417188095590464325 ) ) ;
#19764 = CARTESIAN_POINT ( 'NONE',  ( 0.000000000000000000, 24.80000000000000426, -4.618802153517000519 ) ) ;
#19765 = ORIENTED_EDGE ( 'NONE', *, *, #10903, .T. ) ;
#19766 = CARTESIAN_POINT ( 'NONE',  ( -2.308536264861000387, 25.47398547997000051, 0.4564140279980999915 ) ) ;
#19767 = CARTESIAN_POINT ( 'NONE',  ( 4.903442944881004628, 14.89392636350999233, 3.684989539199001296 ) ) ;
#19768 = EDGE_CURVE ( 'NONE', #11438, #13125, #21324, .T. ) ;
#19769 = CARTESIAN_POINT ( 'NONE',  ( 1.401856813186208361, 12.86851491854003449, 6.537411608044383371 ) ) ;
#19770 = CARTESIAN_POINT ( 'NONE',  ( 19.75000000000000000, -1.659811535170000019, 9.026773995975998943 ) ) ;
#19771 = CARTESIAN_POINT ( 'NONE',  ( 13.50000000000000000, 2.048741218006000064, 10.08990150394999930 ) ) ;
#19772 = CARTESIAN_POINT ( 'NONE',  ( -6.042815832213999983, 16.39253418350000047, -0.9999999878869999526 ) ) ;
#19773 = EDGE_LOOP ( 'NONE', ( #7139, #4158, #8745 ) ) ;
#19774 = DIRECTION ( 'NONE',  ( 0.000000000000000000, 0.000000000000000000, -1.000000000000000000 ) ) ;
#19775 = AXIS2_PLACEMENT_3D ( 'NONE', #6790, #10800, #14061 ) ;
#19776 = CARTESIAN_POINT ( 'NONE',  ( -0.7632405811354259217, 26.22308743037562095, 1.985132959746883641 ) ) ;
#19777 = DIRECTION ( 'NONE',  ( 0.000000000000000000, 1.000000000000000000, 0.000000000000000000 ) ) ;
#19778 = VERTEX_POINT ( 'NONE', #6545 ) ;
#19779 = CARTESIAN_POINT ( 'NONE',  ( -21.11865610815000238, -7.328638157174999890, 7.800684107840000436 ) ) ;
#19780 = CARTESIAN_POINT ( 'NONE',  ( 11.50000000000000000, -7.000000000000000000, 0.000000000000000000 ) ) ;
#19781 = CARTESIAN_POINT ( 'NONE',  ( 15.23271754047294557, 4.697833125319701431, 9.209713511118009066 ) ) ;
#19782 = PLANE ( 'NONE',  #14869 ) ;
#19783 = EDGE_CURVE ( 'NONE', #3685, #20723, #578, .T. ) ;
#19784 = CARTESIAN_POINT ( 'NONE',  ( -2.034154838984999714, 30.92025618834000156, 0.4889338487552999934 ) ) ;
#19785 = CARTESIAN_POINT ( 'NONE',  ( -22.75389368601540951, 1.211706322581030504, 9.258003830841628812 ) ) ;
#19786 = ADVANCED_FACE ( 'NONE', ( #15246 ), #722, .F. ) ;
#19787 = CARTESIAN_POINT ( 'NONE',  ( 4.738215136157003293, 12.61383557389999766, 0.1055552163494999779 ) ) ;
#19788 = ORIENTED_EDGE ( 'NONE', *, *, #10008, .T. ) ;
#19789 = CARTESIAN_POINT ( 'NONE',  ( -21.99722087121331526, -5.675724701917319592, -7.385631801182315215 ) ) ;
#19790 = EDGE_LOOP ( 'NONE', ( #16526, #8579, #11214, #9807 ) ) ;
#19791 = DIRECTION ( 'NONE',  ( 0.000000000000000000, 1.000000000000000000, 0.000000000000000000 ) ) ;
#19792 = CARTESIAN_POINT ( 'NONE',  ( 8.124934037954998800, 10.59999999999999964, 0.000000000000000000 ) ) ;
#19793 = ORIENTED_EDGE ( 'NONE', *, *, #42, .T. ) ;
#19794 = CARTESIAN_POINT ( 'NONE',  ( 11.06619116163224170, -10.57612823871417973, -6.681605107878366923 ) ) ;
#19795 = EDGE_CURVE ( 'NONE', #15508, #19254, #4662, .T. ) ;
#19796 = CARTESIAN_POINT ( 'NONE',  ( 12.00000000000000000, 3.318092558720092899, -8.344102286361790632 ) ) ;
#19797 = EDGE_CURVE ( 'NONE', #11336, #12531, #12613, .T. ) ;
#19798 = CARTESIAN_POINT ( 'NONE',  ( 17.94122805071000215, 6.114706615795999944, -9.275782954962000559 ) ) ;
#19799 = CARTESIAN_POINT ( 'NONE',  ( 19.04006424931000296, -6.376715009848999749, 8.397789983599000863 ) ) ;
#19800 = EDGE_LOOP ( 'NONE', ( #5887, #3916, #21862 ) ) ;
#19801 = CARTESIAN_POINT ( 'NONE',  ( -9.400026492921000454, -14.37830284610000042, 2.006256508544999484 ) ) ;
#19802 = DIRECTION ( 'NONE',  ( 0.000000000000000000, 0.000000000000000000, 1.000000000000000000 ) ) ;
#19803 = CARTESIAN_POINT ( 'NONE',  ( 3.316314694148171149, 24.62756664670258644, -2.704122461039530023 ) ) ;
#19804 = ORIENTED_EDGE ( 'NONE', *, *, #3047, .T. ) ;
#19805 = FACE_OUTER_BOUND ( 'NONE', #12896, .T. ) ;
#19806 = CARTESIAN_POINT ( 'NONE',  ( 21.38215989470702993, -4.982371934643452960, -9.480591854900188409 ) ) ;
#19807 = CARTESIAN_POINT ( 'NONE',  ( -2.817565069457256932, 26.44682129341587995, 2.992080202207100470 ) ) ;
#19808 = CARTESIAN_POINT ( 'NONE',  ( 16.78527092655545516, 10.20993882797034580, 1.972386044144941231 ) ) ;
#19809 = DIRECTION ( 'NONE',  ( 0.000000000000000000, 1.000000000000000000, 0.000000000000000000 ) ) ;
#19810 = CARTESIAN_POINT ( 'NONE',  ( -0.7072731918244000715, 30.87462362680000183, -2.070837331812999782 ) ) ;
#19811 = B_SPLINE_CURVE_WITH_KNOTS ( 'NONE', 3,
 ( #14192, #17838, #21340, #15872 ),
 .UNSPECIFIED., .F., .F.,
 ( 4, 4 ),
 ( 0.000000000000000000, 1.000000000000000000 ),
 .UNSPECIFIED. ) ;
#19812 = CARTESIAN_POINT ( 'NONE',  ( -12.00000000000000000, 7.000000000000000000, 0.000000000000000000 ) ) ;
#19813 = CARTESIAN_POINT ( 'NONE',  ( 0.8452009350949196698, 29.95273695107458067, -1.987689021054610317 ) ) ;
#19814 = EDGE_LOOP ( 'NONE', ( #1144, #13841, #21564, #6096 ) ) ;
#19815 = CARTESIAN_POINT ( 'NONE',  ( 23.73993940136630698, -9.222267920518611106, 1.215187501975043327 ) ) ;
#19816 = CARTESIAN_POINT ( 'NONE',  ( 11.59051697471513442, 12.65550321735096340, -3.079847694010941606 ) ) ;
#19817 = CARTESIAN_POINT ( 'NONE',  ( 4.000000000000060396, 28.25094615492120198, -2.107036910272262809 ) ) ;
#19818 = DIRECTION ( 'NONE',  ( -1.000000000000000000, 0.000000000000000000, 0.000000000000000000 ) ) ;
#19819 = VERTEX_POINT ( 'NONE', #12004 ) ;
#19820 = DIRECTION ( 'NONE',  ( -1.000000000000000000, 0.000000000000000000, 0.000000000000000000 ) ) ;
#19821 = CARTESIAN_POINT ( 'NONE',  ( -5.158992055378997854, 13.96222552554998764, 5.500780647236995335 ) ) ;
#19822 = CARTESIAN_POINT ( 'NONE',  ( 4.942230045011000605, 12.51340480292000024, 0.1092162673837999420 ) ) ;
#19823 = VERTEX_POINT ( 'NONE', #842 ) ;
#19824 = LINE ( 'NONE', #16403, #1075 ) ;
#19825 = ORIENTED_EDGE ( 'NONE', *, *, #678, .F. ) ;
#19826 = PLANE ( 'NONE',  #18725 ) ;
#19827 = SHAPE_DEFINITION_REPRESENTATION ( #16923, #20207 ) ;
#19828 = CARTESIAN_POINT ( 'NONE',  ( -23.75856372112270520, -13.93375672973999890, -0.09623564068393683502 ) ) ;
#19829 = VERTEX_POINT ( 'NONE', #10182 ) ;
#19830 = CARTESIAN_POINT ( 'NONE',  ( -4.080056528100000079, 26.50000000000000000, 4.563746053395999702 ) ) ;
#19831 = CARTESIAN_POINT ( 'NONE',  ( -12.34499313601000026, 9.613013645102999050, -12.04164784824000023 ) ) ;
#19832 = CARTESIAN_POINT ( 'NONE',  ( -23.95495283385999841, -2.336932850305999843, 9.912667528692999497 ) ) ;
#19833 = CARTESIAN_POINT ( 'NONE',  ( -16.91402600854999960, 5.062459437026999964, 8.979130132666000463 ) ) ;
#19834 = CARTESIAN_POINT ( 'NONE',  ( -6.313141446900004894, 16.43093356584002862, 1.007231585192000400 ) ) ;
#19835 = CARTESIAN_POINT ( 'NONE',  ( -22.98062309160115291, -9.860450425915699313, -3.810151497938129683 ) ) ;
#19836 = CARTESIAN_POINT ( 'NONE',  ( 1.986040474371530085, 27.34694121629901886, 0.9569010413172605034 ) ) ;
#19837 = CYLINDRICAL_SURFACE ( 'NONE', #22790, 12.44999999999999929 ) ;
#19838 = FACE_OUTER_BOUND ( 'NONE', #6621, .T. ) ;
#19839 = ORIENTED_EDGE ( 'NONE', *, *, #10719, .T. ) ;
#19840 = CARTESIAN_POINT ( 'NONE',  ( 23.54441667850668551, 2.130327776482009661, 9.046710258410779915 ) ) ;
#19841 = CARTESIAN_POINT ( 'NONE',  ( 1.750000000000000000, 7.000000000000000000, 0.000000000000000000 ) ) ;
#19842 = CARTESIAN_POINT ( 'NONE',  ( 2.445091418594000032, 26.66663313895000087, -0.3381971108622000011 ) ) ;
#19843 = AXIS2_PLACEMENT_3D ( 'NONE', #6677, #21821, #20129 ) ;
#19844 = CARTESIAN_POINT ( 'NONE',  ( -1.923654546119000219, 27.89937716036000381, 1.516486965307999979 ) ) ;
#19845 = DIRECTION ( 'NONE',  ( -1.000000000000000000, 0.000000000000000000, 0.000000000000000000 ) ) ;
#19846 = ORIENTED_EDGE ( 'NONE', *, *, #9515, .F. ) ;
#19847 = DIRECTION ( 'NONE',  ( -0.9996708941621513800, 0.02565352539212875996, 1.659533453806920987E-14 ) ) ;
#19848 = CARTESIAN_POINT ( 'NONE',  ( 3.033043484777522281, 11.87036368078775617, -3.754604677876629548 ) ) ;
#19849 = LINE ( 'NONE', #16317, #20397 ) ;
#19850 = CARTESIAN_POINT ( 'NONE',  ( 11.58073079862069221, -6.605128734743197505, -6.105076039591643244 ) ) ;
#19851 = ORIENTED_EDGE ( 'NONE', *, *, #3091, .T. ) ;
#19852 = ADVANCED_FACE ( 'NONE', ( #15370 ), #13439, .T. ) ;
#19853 = CARTESIAN_POINT ( 'NONE',  ( -7.034000000000000696, 1.310788454998999989E-14, 0.000000000000000000 ) ) ;
#19854 = DIRECTION ( 'NONE',  ( 0.000000000000000000, -1.000000000000000000, 0.000000000000000000 ) ) ;
#19855 = AXIS2_PLACEMENT_3D ( 'NONE', #9481, #17104, #1978 ) ;
#19856 = CARTESIAN_POINT ( 'NONE',  ( 12.51562642131000125, 9.466654096131000173, 1.662047859332999922 ) ) ;
#19857 = CARTESIAN_POINT ( 'NONE',  ( 18.81849951495625106, 6.078002649393266843, 8.477670823501638253 ) ) ;
#19858 = EDGE_LOOP ( 'NONE', ( #5337, #11685, #11553, #17942 ) ) ;
#19859 = CARTESIAN_POINT ( 'NONE',  ( 5.180641154517307001, 13.94961545970955186, 4.027129678755727582 ) ) ;
#19860 = CARTESIAN_POINT ( 'NONE',  ( -1.418793962560999988, 30.13200156660999696, -1.863054310995999829 ) ) ;
#19861 = FACE_OUTER_BOUND ( 'NONE', #6316, .T. ) ;
#19862 = CARTESIAN_POINT ( 'NONE',  ( 13.49999999999999822, -9.686451367697159753, 0.6268225021301814248 ) ) ;
#19863 = ORIENTED_EDGE ( 'NONE', *, *, #23465, .T. ) ;
#19864 = CARTESIAN_POINT ( 'NONE',  ( 0.000000000000000000, 22.00000000000000000, 0.000000000000000000 ) ) ;
#19865 = FACE_OUTER_BOUND ( 'NONE', #3454, .T. ) ;
#19866 = DIRECTION ( 'NONE',  ( -1.000000000000000000, 0.000000000000000000, 0.000000000000000000 ) ) ;
#19867 = ADVANCED_FACE ( 'NONE', ( #4739 ), #19162, .T. ) ;
#19868 = CARTESIAN_POINT ( 'NONE',  ( -23.79921766892433510, -7.721186627919117029, 5.741329154560525616 ) ) ;
#19869 = CARTESIAN_POINT ( 'NONE',  ( 14.69879627327239824, 10.34603584791903508, -0.7108216309658257348 ) ) ;
#19870 = CARTESIAN_POINT ( 'NONE',  ( -2.000000000000000000, 24.50000000000000000, 3.464101615137999968 ) ) ;
#19871 = DIRECTION ( 'NONE',  ( -1.000000000000000000, 0.000000000000000000, 0.000000000000000000 ) ) ;
#19872 = CARTESIAN_POINT ( 'NONE',  ( 0.000000000000000000, -1.550000000000000044, 0.000000000000000000 ) ) ;
#19873 = ORIENTED_EDGE ( 'NONE', *, *, #7583, .F. ) ;
#19874 = LINE ( 'NONE', #12605, #17992 ) ;
#19875 = CIRCLE ( 'NONE', #4783, 1.750000000000000444 ) ;
#19876 = LINE ( 'NONE', #11020, #4991 ) ;
#19877 = ORIENTED_EDGE ( 'NONE', *, *, #23467, .F. ) ;
#19878 = CARTESIAN_POINT ( 'NONE',  ( 0.4021391122705000321, 24.53436591766000063, -2.513213003584999772 ) ) ;
#19879 = CARTESIAN_POINT ( 'NONE',  ( 13.65000000000000036, 1.057482511063999969E-14, 0.000000000000000000 ) ) ;
#19880 = CARTESIAN_POINT ( 'NONE',  ( 11.36701043059877847, -2.759410678255084015, -12.49996441860402463 ) ) ;
#19881 = VECTOR ( 'NONE', #18355, 1000.000000000000000 ) ;
#19882 = CARTESIAN_POINT ( 'NONE',  ( 19.28616666666667712, 9.166202760740587152, 1.338597607047040894 ) ) ;
#19883 = CARTESIAN_POINT ( 'NONE',  ( 2.500000000000000000, 27.61666666666666714, -0.3272492347489370235 ) ) ;
#19884 = EDGE_CURVE ( 'NONE', #7890, #4095, #21106, .T. ) ;
#19885 = CARTESIAN_POINT ( 'NONE',  ( -0.9242717917835999719, 23.66000000000000014, -1.952260652400999996 ) ) ;
#19886 = ORIENTED_EDGE ( 'NONE', *, *, #946, .T. ) ;
#19887 = CARTESIAN_POINT ( 'NONE',  ( 0.6543697108982093891, 30.06753006952333607, 2.434931691670787490 ) ) ;
#19888 = DIRECTION ( 'NONE',  ( 0.000000000000000000, -0.8975663802247816347, -0.4408793407386908392 ) ) ;
#19889 = DIRECTION ( 'NONE',  ( -1.000000000000000000, 0.000000000000000000, 0.000000000000000000 ) ) ;
#19890 = ORIENTED_EDGE ( 'NONE', *, *, #17073, .T. ) ;
#19891 = CARTESIAN_POINT ( 'NONE',  ( -23.51779040664999698, 10.29309294087000026, 3.164445037656999915 ) ) ;
#19892 = CARTESIAN_POINT ( 'NONE',  ( 20.86904166666665716, 7.362300873902134946, -5.658112305383654395 ) ) ;
#19893 = CARTESIAN_POINT ( 'NONE',  ( 14.54704717614944798, 2.944910552188379160, -9.893351561282216267 ) ) ;
#19894 = CARTESIAN_POINT ( 'NONE',  ( -3.000000000000000000, 16.89999999999999858, 0.000000000000000000 ) ) ;
#19895 = CARTESIAN_POINT ( 'NONE',  ( 21.55623526383000055, 5.754856272286999364, -9.648219475427001868 ) ) ;
#19896 = CARTESIAN_POINT ( 'NONE',  ( -2.070379988957000261, 30.04886011138000157, 1.133895954157000174 ) ) ;
#19897 = EDGE_CURVE ( 'NONE', #14474, #10297, #11642, .T. ) ;
#19898 = CARTESIAN_POINT ( 'NONE',  ( 13.60028472826950541, 6.915518368012416595, -5.791054742020698143 ) ) ;
#19899 = CARTESIAN_POINT ( 'NONE',  ( -2.101269504238999275, 11.75436161677999536, -4.249028463402999556 ) ) ;
#19900 = VERTEX_POINT ( 'NONE', #13679 ) ;
#19901 = CARTESIAN_POINT ( 'NONE',  ( -14.00000000000000000, -8.319952449050001420, 6.066771132503999020 ) ) ;
#19902 = VERTEX_POINT ( 'NONE', #22638 ) ;
#19903 = AXIS2_PLACEMENT_3D ( 'NONE', #18472, #1883, #3478 ) ;
#19904 = DIRECTION ( 'NONE',  ( 0.000000000000000000, -1.000000000000000000, 0.000000000000000000 ) ) ;
#19905 = FACE_OUTER_BOUND ( 'NONE', #691, .T. ) ;
#19906 = ADVANCED_FACE ( 'NONE', ( #22882 ), #17572, .T. ) ;
#19907 = EDGE_LOOP ( 'NONE', ( #2084, #15063, #19638 ) ) ;
#19908 = DIRECTION ( 'NONE',  ( -0.9063077870366409439, 0.000000000000000000, 0.4226182617407191477 ) ) ;
#19909 = CARTESIAN_POINT ( 'NONE',  ( 10.35615758860000035, 0.000000000000000000, 0.000000000000000000 ) ) ;
#19910 = DIRECTION ( 'NONE',  ( -1.000000000000000000, 0.000000000000000000, 0.000000000000000000 ) ) ;
#19911 = CIRCLE ( 'NONE', #19123, 1.000000000000000666 ) ;
#19912 = CARTESIAN_POINT ( 'NONE',  ( 24.50000000000000000, 4.174438572590999431E-14, -12.50000000000000000 ) ) ;
#19913 = EDGE_CURVE ( 'NONE', #6330, #20095, #8742, .T. ) ;
#19914 = EDGE_CURVE ( 'NONE', #17699, #21250, #13601, .T. ) ;
#19915 = ORIENTED_EDGE ( 'NONE', *, *, #17973, .F. ) ;
#19916 = CARTESIAN_POINT ( 'NONE',  ( -8.883540065846000644, 13.80244821480000006, -4.188663184106999893 ) ) ;
#19917 = CARTESIAN_POINT ( 'NONE',  ( 13.49999999999999822, 7.584517159776716255, 6.431457497586518635 ) ) ;
#19918 = DIRECTION ( 'NONE',  ( 0.000000000000000000, 0.000000000000000000, 1.000000000000000000 ) ) ;
#19919 = ORIENTED_EDGE ( 'NONE', *, *, #8615, .T. ) ;
#19920 = FILL_AREA_STYLE ('',( #7073 ) ) ;
#19921 = CARTESIAN_POINT ( 'NONE',  ( 23.29410800009176796, -1.498401570910810054, -10.49305455072095228 ) ) ;
#19922 = CARTESIAN_POINT ( 'NONE',  ( -5.372793533988000192, 16.07374366253000275, 2.940837684191000001 ) ) ;
#19923 = CARTESIAN_POINT ( 'NONE',  ( 17.44105274156537533, -8.133647787183173605, 6.538978001247210514 ) ) ;
#19924 = CARTESIAN_POINT ( 'NONE',  ( -17.54351602131999854, -8.091578619838001529, 7.581262777877999959 ) ) ;
#19925 = CARTESIAN_POINT ( 'NONE',  ( 0.1890102160836000245, 30.42465970005999765, 2.335336163465000059 ) ) ;
#19926 = ADVANCED_FACE ( 'NONE', ( #21803 ), #10680, .F. ) ;
#19927 = AXIS2_PLACEMENT_3D ( 'NONE', #1747, #14576, #1394 ) ;
#19928 = CARTESIAN_POINT ( 'NONE',  ( -16.36737399056000086, -1.805578197078999914, -9.588658350757999216 ) ) ;
#19929 = CARTESIAN_POINT ( 'NONE',  ( 1.691637037686638312, 29.88931209851202908, -1.343040514645775341 ) ) ;
#19930 = ORIENTED_EDGE ( 'NONE', *, *, #12341, .T. ) ;
#19931 = CARTESIAN_POINT ( 'NONE',  ( 11.43887872963139252, 12.36312605253445085, -3.586317572249483998 ) ) ;
#19932 = CARTESIAN_POINT ( 'NONE',  ( 23.59056163660901717, 2.084868816671024305, -10.39936085362623075 ) ) ;
#19933 = CARTESIAN_POINT ( 'NONE',  ( 11.74999999482999868, 0.000000000000000000, 1.045589212608000028E-14 ) ) ;
#19934 = ORIENTED_EDGE ( 'NONE', *, *, #2121, .T. ) ;
#19935 = CARTESIAN_POINT ( 'NONE',  ( 19.24399999999999977, 9.165120680968000144, 0.000000000000000000 ) ) ;
#19936 = CARTESIAN_POINT ( 'NONE',  ( 4.905991498448432075, 14.36426274116703183, -3.820313869637216975 ) ) ;
#19937 = CARTESIAN_POINT ( 'NONE',  ( 4.670439692284003463, 12.43658471589000492, -1.070905091827999867 ) ) ;
#19938 = ORIENTED_EDGE ( 'NONE', *, *, #13392, .F. ) ;
#19939 = CARTESIAN_POINT ( 'NONE',  ( 18.08325125730999972, 1.019414021290000028, 9.192347282599000025 ) ) ;
#19940 = ORIENTED_EDGE ( 'NONE', *, *, #9672, .T. ) ;
#19941 = CONICAL_SURFACE ( 'NONE', #22615, 9.152445778720998959, 0.02565634000431304615 ) ;
#19942 = CARTESIAN_POINT ( 'NONE',  ( 1.499758741878467250, 26.53402357736653627, -1.612855151721995117 ) ) ;
#19943 = CONTEXT_DEPENDENT_SHAPE_REPRESENTATION ( #273, #14980 ) ;
#19944 = CARTESIAN_POINT ( 'NONE',  ( 0.000000000000000000, 26.50000000000000355, 0.000000000000000000 ) ) ;
#19945 = VERTEX_POINT ( 'NONE', #16227 ) ;
#19946 = CARTESIAN_POINT ( 'NONE',  ( -19.37239492268833629, 7.702177344478975840, 5.087202664328104973 ) ) ;
#19947 = CARTESIAN_POINT ( 'NONE',  ( 12.05662674931000033, -10.44547366770999908, -0.2303471896619999904 ) ) ;
#19948 = CARTESIAN_POINT ( 'NONE',  ( -24.27612620378999964, 7.862241769065999364, 6.487233881142000058 ) ) ;
#19949 = CARTESIAN_POINT ( 'NONE',  ( -15.76129435812999979, 9.303360818536997812, -2.884552524785000127 ) ) ;
#19951 = EDGE_CURVE ( 'NONE', #18160, #11418, #6782, .T. ) ;
#19950 = DIRECTION ( 'NONE',  ( 0.000000000000000000, 1.000000000000000000, 0.000000000000000000 ) ) ;
#19952 = EDGE_CURVE ( 'NONE', #18848, #9480, #204, .T. ) ;
#19953 = CARTESIAN_POINT ( 'NONE',  ( -22.82621233711391895, -6.539040155037235458, -8.301165428859656359 ) ) ;
#19954 = CARTESIAN_POINT ( 'NONE',  ( 1.787816191774978414, 26.68441241925206597, -1.290061143064831883 ) ) ;
#19955 = CARTESIAN_POINT ( 'NONE',  ( -1.864615697012000028, 27.95000240010000070, -2.183184479328999839 ) ) ;
#19956 = CARTESIAN_POINT ( 'NONE',  ( 1.712608848029143926, 30.68724016082039796, -1.316683541910883104 ) ) ;
#19957 = ORIENTED_EDGE ( 'NONE', *, *, #22692, .F. ) ;
#19958 = CARTESIAN_POINT ( 'NONE',  ( 12.52688711657000020, -6.216878364870000340, 12.50000000000000000 ) ) ;
#19959 = LINE ( 'NONE', #14612, #3831 ) ;
#19960 = CARTESIAN_POINT ( 'NONE',  ( 0.4858445502738999999, 28.31619850838000119, -2.214344957515000267 ) ) ;
#19961 = CIRCLE ( 'NONE', #20327, 5.000000000000000000 ) ;
#19962 = CARTESIAN_POINT ( 'NONE',  ( -1.662740336262000129, 27.11937716036000268, 1.798742361870000028 ) ) ;
#19963 = CARTESIAN_POINT ( 'NONE',  ( 18.93264468355999952, 0.000000000000000000, 0.000000000000000000 ) ) ;
#19964 = ORIENTED_EDGE ( 'NONE', *, *, #3894, .T. ) ;
#19965 = CARTESIAN_POINT ( 'NONE',  ( 18.03466666666665574, -4.599982198591594518, 7.981289300288839428 ) ) ;
#19966 = CARTESIAN_POINT ( 'NONE',  ( 4.443184208718807149, 12.29965960042665962, -1.929093012512449912 ) ) ;
#19967 = CARTESIAN_POINT ( 'NONE',  ( 3.150855693196132457, 28.10222989789001602, 2.799640769041085164 ) ) ;
#19968 = CARTESIAN_POINT ( 'NONE',  ( 11.62486552301403897, -5.600815039373708615, -7.038964122195418227 ) ) ;
#19969 = ORIENTED_EDGE ( 'NONE', *, *, #18731, .T. ) ;
#19970 = CARTESIAN_POINT ( 'NONE',  ( -0.6543697108981503252, 24.16666666666667140, 2.434931691670802145 ) ) ;
#19971 = CARTESIAN_POINT ( 'NONE',  ( 0.000000000000000000, 26.50000000000000355, 0.000000000000000000 ) ) ;
#19972 = AXIS2_PLACEMENT_3D ( 'NONE', #5904, #13290, #9078 ) ;
#19973 = B_SPLINE_CURVE_WITH_KNOTS ( 'NONE', 3,
 ( #18815, #22097, #11325, #3690, #277, #18698, #7681, #14814, #2107, #7431, #20636, #9496 ),
 .UNSPECIFIED., .F., .F.,
 ( 4, 1, 1, 1, 1, 2, 2, 4 ),
 ( 0.000000000000000000, 0.2499999999999996114, 0.3749999999999996114, 0.4374999999999996669, 0.4687499999999997224, 0.4843749999999997224, 0.4999999999999997780, 1.000000000000000000 ),
 .UNSPECIFIED. ) ;
#19974 = CARTESIAN_POINT ( 'NONE',  ( 12.07687642131000061, 2.140746470509000243, -9.358182000212998730 ) ) ;
#19975 = CARTESIAN_POINT ( 'NONE',  ( 18.70306232122398526, 8.883973405854113992, 5.460658337303971877 ) ) ;
#19976 = VERTEX_POINT ( 'NONE', #12485 ) ;
#19977 = CARTESIAN_POINT ( 'NONE',  ( 3.999702431745993270, 28.00639765414744886, 0.3779811684581091957 ) ) ;
#19978 = CARTESIAN_POINT ( 'NONE',  ( 0.7871505218098000523, 29.20548547997000099, -2.205525275559999887 ) ) ;
#19979 = CARTESIAN_POINT ( 'NONE',  ( -12.51567934522000058, 6.525107353416999878, -6.187672237275999798 ) ) ;
#19980 = CARTESIAN_POINT ( 'NONE',  ( 13.49999999999999822, -8.028714044826315899, 6.032243616578709222 ) ) ;
#19981 = ORIENTED_EDGE ( 'NONE', *, *, #19155, .T. ) ;
#19982 = AXIS2_PLACEMENT_3D ( 'NONE', #13604, #770, #8170 ) ;
#19983 = DIRECTION ( 'NONE',  ( 1.000000000000000000, 0.000000000000000000, 0.000000000000000000 ) ) ;
#19984 = CARTESIAN_POINT ( 'NONE',  ( -23.74465998031000069, -13.93375672974000068, 0.8660254037843999608 ) ) ;
#19985 = CARTESIAN_POINT ( 'NONE',  ( 2.949999988794999695, 24.49999998879500041, 5.832342955284000153E-08 ) ) ;
#19986 = CARTESIAN_POINT ( 'NONE',  ( -4.649999999999999467, 17.00000000000000000, 0.000000000000000000 ) ) ;
#19987 = CARTESIAN_POINT ( 'NONE',  ( -3.649794085728322202, 24.70197603011190424, 2.511592555635381974 ) ) ;
#19988 = CARTESIAN_POINT ( 'NONE',  ( 2.948934117662000087, 11.89081811946000933, 3.984846700880998682 ) ) ;
#19989 = EDGE_CURVE ( 'NONE', #3305, #5391, #1341, .T. ) ;
#19990 = CARTESIAN_POINT ( 'NONE',  ( -7.834000000000000519, 10.69999999999999929, 0.000000000000000000 ) ) ;
#19991 = VERTEX_POINT ( 'NONE', #18056 ) ;
#19992 = CARTESIAN_POINT ( 'NONE',  ( -1.409459525220179810, 30.51584936511932611, 2.103659993609944490 ) ) ;
#19993 = AXIS2_PLACEMENT_3D ( 'NONE', #1136, #12522, #19908 ) ;
#19994 = DIRECTION ( 'NONE',  ( 0.000000000000000000, 0.000000000000000000, -1.000000000000000000 ) ) ;
#19995 = EDGE_LOOP ( 'NONE', ( #3747, #1697, #18402, #5665 ) ) ;
#19996 = CARTESIAN_POINT ( 'NONE',  ( 2.285327255250000356, 25.99744178769000058, -0.8000105884810000401 ) ) ;
#19997 = CARTESIAN_POINT ( 'NONE',  ( 0.000000000000000000, -1.550000000000000044, 0.000000000000000000 ) ) ;
#19998 = CARTESIAN_POINT ( 'NONE',  ( 11.55284350193982235, -3.530773253025947689, -12.49989659317496837 ) ) ;
#19999 = CARTESIAN_POINT ( 'NONE',  ( 19.53916666666666302, 4.841071979630906519, 7.905488166010842477 ) ) ;
#20000 = FACE_OUTER_BOUND ( 'NONE', #8803, .T. ) ;
#20001 = AXIS2_PLACEMENT_3D ( 'NONE', #12547, #23560, #16521 ) ;
#20002 = ORIENTED_EDGE ( 'NONE', *, *, #5430, .F. ) ;
#20003 = CARTESIAN_POINT ( 'NONE',  ( -15.14859190273999801, -7.578844389069999465, 6.091136938512000221 ) ) ;
#20004 = AXIS2_PLACEMENT_3D ( 'NONE', #8711, #6640, #12466 ) ;
#20005 = CARTESIAN_POINT ( 'NONE',  ( 1.699986957659999964, 9.000014576061998284, -0.8485216275457999613 ) ) ;
#20006 = ORIENTED_EDGE ( 'NONE', *, *, #1276, .T. ) ;
#20007 = CARTESIAN_POINT ( 'NONE',  ( -24.78987924950000021, -10.60142683737000091, 1.295814263090999896 ) ) ;
#20008 = AXIS2_PLACEMENT_3D ( 'NONE', #12951, #10914, #23852 ) ;
#20009 = CARTESIAN_POINT ( 'NONE',  ( -1.018972323971000016, 25.15353811475999990, -1.887072216533999924 ) ) ;
#20010 = CARTESIAN_POINT ( 'NONE',  ( 14.42486780284139058, -1.324147059350222921, -10.23272323601588596 ) ) ;
#20011 = CARTESIAN_POINT ( 'NONE',  ( 0.000000000000000000, 28.00000000000000000, 0.000000000000000000 ) ) ;
#20012 = CARTESIAN_POINT ( 'NONE',  ( 22.62059167554999917, -6.125430812571999617, 9.452137327804999600 ) ) ;
#20013 = CARTESIAN_POINT ( 'NONE',  ( -2.042556580646999631, 30.83875785297000149, 0.9163512981227001086 ) ) ;
#20014 = DIRECTION ( 'NONE',  ( -1.000000000000000000, 0.000000000000000000, 0.000000000000000000 ) ) ;
#20015 = CARTESIAN_POINT ( 'NONE',  ( -4.528963122208002900, 12.53559761094001423, -1.650262910948000927 ) ) ;
#20016 = B_SPLINE_CURVE_WITH_KNOTS ( 'NONE', 3,
 ( #22394, #16939, #5684, #9325, #13070, #11142, #15228, #11386, #16699, #9680, #1937, #20469, #7495, #3877, #15111, #13188, #342, #9794 ),
 .UNSPECIFIED., .F., .F.,
 ( 4, 2, 2, 2, 2, 2, 2, 2, 4 ),
 ( 0.000000000000000000, 0.1250000000000000000, 0.2500000000000000000, 0.3750000000000000000, 0.5000000000000000000, 0.6250000000000000000, 0.7500000000000000000, 0.8750000000000000000, 1.000000000000000000 ),
 .UNSPECIFIED. ) ;
#20017 = CARTESIAN_POINT ( 'NONE',  ( -21.35476253787999923, 9.219287007783998789, 0.000000000000000000 ) ) ;
#20018 = ADVANCED_FACE ( 'NONE', ( #6906 ), #14299, .F. ) ;
#20019 = VERTEX_POINT ( 'NONE', #21446 ) ;
#20020 = CARTESIAN_POINT ( 'NONE',  ( -1.536366799937290084, 29.48333333333333428, -1.999167105995448113 ) ) ;
#20021 = DIRECTION ( 'NONE',  ( 0.000000000000000000, 0.000000000000000000, 1.000000000000000000 ) ) ;
#20022 = AXIS2_PLACEMENT_3D ( 'NONE', #17090, #3904, #22298 ) ;
#20023 = B_SPLINE_CURVE_WITH_KNOTS ( 'NONE', 3,
 ( #4855, #8603, #21565, #8726, #6777, #14169 ),
 .UNSPECIFIED., .F., .F.,
 ( 4, 2, 4 ),
 ( 0.002491295001356702652, 0.003048372566543609916, 0.003605450131730517181 ),
 .UNSPECIFIED. ) ;
#20024 = ORIENTED_EDGE ( 'NONE', *, *, #9047, .F. ) ;
#20025 = DIRECTION ( 'NONE',  ( 0.000000000000000000, 0.000000000000000000, 1.000000000000000000 ) ) ;
#20026 = CARTESIAN_POINT ( 'NONE',  ( 16.67416666666665392, -7.950782698768437129, -4.582399293024413289 ) ) ;
#20027 = AXIS2_PLACEMENT_3D ( 'NONE', #22134, #11117, #12816 ) ;
#20028 = CARTESIAN_POINT ( 'NONE',  ( 12.00000000000000000, 5.273090321616999532, -7.267806174758000282 ) ) ;
#20029 = CARTESIAN_POINT ( 'NONE',  ( 14.69311188949999902, 10.43397013479000002, 3.548706328086999928 ) ) ;
#20030 = AXIS2_PLACEMENT_3D ( 'NONE', #14129, #15927, #17894 ) ;
#20031 = EDGE_CURVE ( 'NONE', #1813, #11130, #6402, .T. ) ;
#20032 = EDGE_LOOP ( 'NONE', ( #2739, #16516, #19028, #16306 ) ) ;
#20033 = CARTESIAN_POINT ( 'NONE',  ( -12.10791923250999957, 4.794444003321999936, -13.75758207492000018 ) ) ;
#20034 = CARTESIAN_POINT ( 'NONE',  ( 13.50000000000000178, 5.145877244135721007, 8.714246119701103410 ) ) ;
#20035 = CARTESIAN_POINT ( 'NONE',  ( -14.40719396494441185, -12.69649082865952927, -3.008800086024487452 ) ) ;
#20036 = ORIENTED_EDGE ( 'NONE', *, *, #3618, .T. ) ;
#20037 = SURFACE_STYLE_USAGE ( .BOTH. , #5037 ) ;
#20038 = CARTESIAN_POINT ( 'NONE',  ( 23.55883927622098639, 7.420590745144572509, -7.577917290854461640 ) ) ;
#20039 = CARTESIAN_POINT ( 'NONE',  ( -14.00000000000000178, -0.8805840824569890479, 9.770682771554191959 ) ) ;
#20040 = CARTESIAN_POINT ( 'NONE',  ( 15.99032225483610148, -8.667267649197352597, -5.673782229705955693 ) ) ;
#20041 = VECTOR ( 'NONE', #3121, 999.9999999999998863 ) ;
#20042 = AXIS2_PLACEMENT_3D ( 'NONE', #20389, #32, #3674 ) ;
#20043 = EDGE_CURVE ( 'NONE', #16445, #7738, #2151, .T. ) ;
#20044 = CARTESIAN_POINT ( 'NONE',  ( -6.142578036165183164, 15.03063358819925810, 3.518293753452066408 ) ) ;
#20045 = CARTESIAN_POINT ( 'NONE',  ( 2.284685590549000000, 28.98591928658000327, 0.5193202084365000637 ) ) ;
#20046 = CARTESIAN_POINT ( 'NONE',  ( -14.94546155477000049, -9.714114572133000891, -0.2583773470232999525 ) ) ;
#20047 = ADVANCED_FACE ( 'NONE', ( #4860 ), #4076, .F. ) ;
#20048 = CARTESIAN_POINT ( 'NONE',  ( 2.036831998448072500, 29.84739247495543779, -0.7268712922005031718 ) ) ;
#20049 = EDGE_LOOP ( 'NONE', ( #15863, #10651, #18972 ) ) ;
#20050 = CARTESIAN_POINT ( 'NONE',  ( 19.33455408719442659, -9.641156592198640851, 4.152421770286800928 ) ) ;
#20051 = DIRECTION ( 'NONE',  ( 1.576486815247195039E-18, 7.363894760761759519E-10, -1.000000000000000000 ) ) ;
#20052 = VERTEX_POINT ( 'NONE', #5672 ) ;
#20053 = CARTESIAN_POINT ( 'NONE',  ( 24.35625626386760700, -9.206804001270699089, -9.053347694469197293 ) ) ;
#20054 = CARTESIAN_POINT ( 'NONE',  ( 5.110054639284849820, 14.01663359027072886, -3.973409363128503458 ) ) ;
#20055 = CIRCLE ( 'NONE', #5357, 0.8000000000000003775 ) ;
#20056 = CARTESIAN_POINT ( 'NONE',  ( 4.761848349162001170, 12.47239002814000131, -0.5119988763560997524 ) ) ;
#20057 = VERTEX_POINT ( 'NONE', #16689 ) ;
#20058 = ADVANCED_FACE ( 'NONE', ( #16574 ), #11257, .T. ) ;
#20059 = DIRECTION ( 'NONE',  ( 0.000000000000000000, 0.000000000000000000, -1.000000000000000000 ) ) ;
#20060 = ORIENTED_EDGE ( 'NONE', *, *, #21265, .T. ) ;
#20061 = CARTESIAN_POINT ( 'NONE',  ( -14.25547409885999883, 6.467346689388999259, -12.35539204541999858 ) ) ;
#20062 = CONTEXT_DEPENDENT_SHAPE_REPRESENTATION ( #20114, #9584 ) ;
#20063 = LINE ( 'NONE', #21992, #6326 ) ;
#20064 = AXIS2_PLACEMENT_3D ( 'NONE', #14753, #14638, #98 ) ;
#20065 = ORIENTED_EDGE ( 'NONE', *, *, #936, .F. ) ;
#20066 = CARTESIAN_POINT ( 'NONE',  ( -19.40606844572667455, 8.247006132493126529, 4.148077805920550531 ) ) ;
#20067 = VECTOR ( 'NONE', #4419, 1000.000000000000227 ) ;
#20068 = AXIS2_PLACEMENT_3D ( 'NONE', #19184, #8173, #8292 ) ;
#20069 = CARTESIAN_POINT ( 'NONE',  ( -22.50967266913999865, 8.778109831006000618, 5.086562693550999548 ) ) ;
#20070 =( BOUNDED_SURFACE ( )  B_SPLINE_SURFACE ( 3, 3, ( 
 ( #9164, #12687, #16540, #16419, #1897 ),
 ( #12905, #11228, #18148, #18607, #20076 ),
 ( #20305, #5526, #8936, #65, #21885 ),
 ( #18484, #2013, #23808, #7451, #20424 ) ),
 .UNSPECIFIED., .F., .F., .T. ) 
 B_SPLINE_SURFACE_WITH_KNOTS ( ( 4, 4 ),
 ( 4, 1, 4 ),
 ( 0.000000000000000000, 1.000000000000000000 ),
 ( 0.9387615814217999954, 0.9657285282888999900, 0.9947468880704000149 ),
 .UNSPECIFIED. ) 
 GEOMETRIC_REPRESENTATION_ITEM ( )  RATIONAL_B_SPLINE_SURFACE ( (
 ( 1.226462146532000030, 1.226462146532000030, 1.226462146532000030, 1.226462146532000030, 1.226462146532000030),
 ( 0.9245126178228000313, 0.9245126178228000313, 0.9245126178228000313, 0.9245126178228000313, 0.9245126178228000313),
 ( 0.9245126178228000313, 0.9245126178228000313, 0.9245126178228000313, 0.9245126178228000313, 0.9245126178228000313),
 ( 1.226462146532000030, 1.226462146532000030, 1.226462146532000030, 1.226462146532000030, 1.226462146532000030) ) ) 
 REPRESENTATION_ITEM ( '' )  SURFACE ( )  );
#20071 = CARTESIAN_POINT ( 'NONE',  ( -18.80824957768000161, -1.381956751031999886, 9.727523358913000351 ) ) ;
#20072 = DIRECTION ( 'NONE',  ( 0.000000000000000000, 0.000000000000000000, 1.000000000000000000 ) ) ;
#20073 = CARTESIAN_POINT ( 'NONE',  ( -24.31884963048089077, 4.568789909715829545, -9.568519739173572347 ) ) ;
#20074 = CARTESIAN_POINT ( 'NONE',  ( -2.169831354736061702, 27.79746079784813162, -0.1190495946757019197 ) ) ;
#20075 = VECTOR ( 'NONE', #8037, 1000.000000000000000 ) ;
#20076 = CARTESIAN_POINT ( 'NONE',  ( -5.790984316780003027, 15.02418496909000112, 3.017193391611002085 ) ) ;
#20077 = EDGE_CURVE ( 'NONE', #23198, #14966, #22256, .T. ) ;
#20078 = CARTESIAN_POINT ( 'NONE',  ( 1.139984784021916608, 30.73313778691811748, -1.836321495231491463 ) ) ;
#20079 = ORIENTED_EDGE ( 'NONE', *, *, #7257, .T. ) ;
#20080 = ADVANCED_FACE ( 'NONE', ( #11375 ), #23964, .T. ) ;
#20081 = CARTESIAN_POINT ( 'NONE',  ( 23.43873132191483322, 5.239923916412018379, 7.729598312681994265 ) ) ;
#20082 = CARTESIAN_POINT ( 'NONE',  ( 1.611535839303107176, 26.30674319040050335, 1.527120279818484194 ) ) ;
#20083 = CARTESIAN_POINT ( 'NONE',  ( 14.93123391489891283, -8.895217880621389739, 1.951093223186516568 ) ) ;
#20084 = CARTESIAN_POINT ( 'NONE',  ( -0.3140912549738999471, 27.77114211382000164, 2.270811333173000435 ) ) ;
#20085 = MECHANICAL_DESIGN_GEOMETRIC_PRESENTATION_REPRESENTATION (  '', ( #8873 ), #12734 ) ;
#20086 = VERTEX_POINT ( 'NONE', #3867 ) ;
#20087 = CARTESIAN_POINT ( 'NONE',  ( -1.299969483453414343, 11.55360400645373709, -4.638995061499023187 ) ) ;
#20088 = CLOSED_SHELL ( 'NONE', ( #11362, #1200, #13246, #19739, #13089, #14450, #7152, #2820, #5113, #15563, #21249, #19236, #15020, #19145, #22411 ) ) ;
#20089 = EDGE_CURVE ( 'NONE', #4654, #21095, #2043, .T. ) ;
#20090 = CARTESIAN_POINT ( 'NONE',  ( 3.824747490998164245, 28.25094615491878614, 2.410583160007404580 ) ) ;
#20091 = B_SPLINE_CURVE_WITH_KNOTS ( 'NONE', 3,
 ( #14391, #23600, #1564, #8950, #4963, #19612, #8837, #6521, #6760, #1068, #21784, #7003, #3021, #19738, #19966, #16316, #12464, #3149, #13907, #4718, #10531, #21548, #17916, #19492, #16072, #23472, #14032, #6881, #3386, #14276, #2898, #15835, #15951, #21671, #5083, #19848, #10648, #10768, #18035, #12223, #18162, #10280, #10408, #17670, #8469, #23225, #21423, #17801, #23344, #12812, #12919, #13160, #9528, #5651, #1668, #13037, #23707, #7351, #11240, #18496, #5309, #14734, #9412, #7228, #11356, #9058, #9298, #10992, #20087, #20202, #2138, #1908, #7114, #3845, #14504, #21898, #14962, #22360, #9175, #12698, #23818, #5776, #16430, #20552, #11112, #10882, #18269, #14620, #3965, #2024, #16671, #18728, #18618, #22016, #16554, #16784, #3609, #3502, #191, #22130, #5429, #23944, #18377, #1787, #78, #7584, #5538, #20315, #3721, #7463, #14847, #22237, #20434, #15321 ),
 .UNSPECIFIED., .F., .F.,
 ( 4, 1, 1, 1, 1, 2, 2, 2, 1, 1, 1, 2, 2, 2, 1, 1, 1, 2, 2, 2, 1, 1, 1, 2, 2, 2, 1, 2, 2, 2, 2, 2, 2, 1, 1, 2, 2, 2, 2, 1, 1, 2, 2, 2, 1, 1, 1, 2, 2, 2, 1, 1, 1, 2, 2, 2, 1, 1, 1, 2, 2, 2, 1, 1, 1, 2, 2, 2, 1, 1, 2, 2, 4 ),
 ( 0.000000000000000000, 0.03125000000000074940, 0.04687500000000113798, 0.05468750000000132533, 0.05859375000000146411, 0.06054687500000152656, 0.06250000000000159595, 0.09375000000000288658, 0.1093750000000035666, 0.1171875000000038858, 0.1210937500000039968, 0.1230468750000041078, 0.1250000000000041911, 0.1562500000000040246, 0.1718750000000038858, 0.1796875000000039413, 0.1835937500000039413, 0.1855468750000038858, 0.1875000000000038580, 0.2187500000000034417, 0.2343750000000032196, 0.2421875000000031086, 0.2460937500000030531, 0.2480468750000029421, 0.2500000000000028311, 0.2656250000000020539, 0.2734375000000016098, 0.2773437500000014433, 0.2812500000000012212, 0.2968750000000006106, 0.3125000000000000000, 0.3437499999999987232, 0.3593749999999980571, 0.3671874999999977796, 0.3710937499999975575, 0.3730468749999975020, 0.3749999999999974465, 0.4062499999999961697, 0.4218749999999955591, 0.4296874999999952816, 0.4335937499999951150, 0.4355468749999950595, 0.4374999999999950040, 0.4687499999999941158, 0.4843749999999937272, 0.4921874999999935607, 0.4960937499999933942, 0.4980468749999933942, 0.4999999999999933942, 0.5312499999999928946, 0.5468749999999926725, 0.5546874999999925615, 0.5585937499999925615, 0.5605468749999924505, 0.5624999999999923395, 0.5937499999999921174, 0.6093749999999920064, 0.6171874999999918954, 0.6210937499999918954, 0.6230468749999920064, 0.6249999999999920064, 0.6874999999999917843, 0.7187499999999918954, 0.7343749999999920064, 0.7421874999999920064, 0.7460937499999921174, 0.7499999999999922284, 0.8124999999999941158, 0.8437499999999952260, 0.8593749999999957812, 0.8671874999999960032, 0.8749999999999963363, 1.000000000000000000 ),
 .UNSPECIFIED. ) ;
#20092 = EDGE_CURVE ( 'NONE', #14850, #2766, #18397, .T. ) ;
#20093 = AXIS2_PLACEMENT_3D ( 'NONE', #21754, #18003, #5167 ) ;
#20094 = CARTESIAN_POINT ( 'NONE',  ( 1.632208092639368724, 6.971545505544572308, 0.6323144000017536515 ) ) ;
#20095 = VERTEX_POINT ( 'NONE', #22039 ) ;
#20096 = CARTESIAN_POINT ( 'NONE',  ( 2.500000000000000000, 24.40000000000000213, 0.000000000000000000 ) ) ;
#20097 = FACE_OUTER_BOUND ( 'NONE', #17726, .T. ) ;
#20098 = CARTESIAN_POINT ( 'NONE',  ( 15.50362658531000193, -9.889101471244000408, -2.495492728532000104 ) ) ;
#20099 = CARTESIAN_POINT ( 'NONE',  ( 18.44061664567739456, 9.767409168246320661, -3.641564553964325324 ) ) ;
#20100 = UNCERTAINTY_MEASURE_WITH_UNIT (LENGTH_MEASURE( 1.000000000000000082E-05 ), #6831, 'distance_accuracy_value', 'NONE');
#20101 = AXIS2_PLACEMENT_3D ( 'NONE', #19909, #11411, #13098 ) ;
#20102 = PLANE ( 'NONE',  #21641 ) ;
#20103 = CARTESIAN_POINT ( 'NONE',  ( -0.3357239997244999552, 28.83046706394999958, 2.247102726245999715 ) ) ;
#20104 = CARTESIAN_POINT ( 'NONE',  ( 0.000000000000000000, 13.10000000000000142, 0.000000000000000000 ) ) ;
#20105 = CARTESIAN_POINT ( 'NONE',  ( 13.50000000000000178, -9.660468571430653739, -0.1198354625297687187 ) ) ;
#20106 = AXIS2_PLACEMENT_3D ( 'NONE', #23586, #2764, #10267 ) ;
#20107 = ORIENTED_EDGE ( 'NONE', *, *, #4806, .F. ) ;
#20108 = CARTESIAN_POINT ( 'NONE',  ( -24.41904027019043255, 11.84953030585170985, 4.475986625696044996 ) ) ;
#20109 = CARTESIAN_POINT ( 'NONE',  ( 19.68770938589000252, -10.68602309994999899, -0.7848986935476999216 ) ) ;
#20110 = CARTESIAN_POINT ( 'NONE',  ( -24.39641198927269983, 7.916710863778032348, -6.620963688920025625 ) ) ;
#20111 = CARTESIAN_POINT ( 'NONE',  ( 24.50000000000000711, -5.724380115368404631, 8.895336411110607244 ) ) ;
#20112 = DIRECTION ( 'NONE',  ( -1.000000000000000000, 0.000000000000000000, 0.000000000000000000 ) ) ;
#20113 = CARTESIAN_POINT ( 'NONE',  ( -4.914666472637005512, 12.43931986496000874, -0.06122609934487997785 ) ) ;
#20114 =( REPRESENTATION_RELATIONSHIP ('NONE','NONE', #13682, #20207 ) REPRESENTATION_RELATIONSHIP_WITH_TRANSFORMATION ( #1766 )SHAPE_REPRESENTATION_RELATIONSHIP( ) );
#20115 = CARTESIAN_POINT ( 'NONE',  ( -0.2348186520982191716, 29.21777802950449043, -2.147017149994515872 ) ) ;
#20116 = CARTESIAN_POINT ( 'NONE',  ( -23.48034867834999773, 8.702766563787999843, 6.962597091951999495 ) ) ;
#20117 = ORIENTED_EDGE ( 'NONE', *, *, #18004, .T. ) ;
#20118 = CARTESIAN_POINT ( 'NONE',  ( 2.321942789092308779, 23.87531119754747522, 0.5770122056809254829 ) ) ;
#20119 = ORIENTED_EDGE ( 'NONE', *, *, #18579, .F. ) ;
#20120 = CIRCLE ( 'NONE', #13912, 2.000000000000000000 ) ;
#20121 = CARTESIAN_POINT ( 'NONE',  ( 0.5283825141746999465, 23.97514525888999870, 2.095676833831000341 ) ) ;
#20122 = CARTESIAN_POINT ( 'NONE',  ( 1.536366799937295413, 28.28333333333333499, 1.999167105995444338 ) ) ;
#20123 = CARTESIAN_POINT ( 'NONE',  ( 4.157699912148990151, 13.38119708362450666, 5.410788887539548675 ) ) ;
#20124 = CARTESIAN_POINT ( 'NONE',  ( 18.91915022178003625, -1.886358478162994956, 10.25880577272608107 ) ) ;
#20125 = CARTESIAN_POINT ( 'NONE',  ( 13.50000000000000355, 1.456528203957302647, 10.21014957686530344 ) ) ;
#20126 = ORIENTED_EDGE ( 'NONE', *, *, #1055, .T. ) ;
#20127 = CARTESIAN_POINT ( 'NONE',  ( -16.57050433853000015, -7.584645295112999897, -6.147042915735999813 ) ) ;
#20128 = AXIS2_PLACEMENT_3D ( 'NONE', #7215, #17017, #14829 ) ;
#20129 = DIRECTION ( 'NONE',  ( -1.000000000000000000, 0.000000000000000000, 0.000000000000000000 ) ) ;
#20130 = FACE_OUTER_BOUND ( 'NONE', #17733, .T. ) ;
#20131 = ORIENTED_EDGE ( 'NONE', *, *, #23639, .F. ) ;
#20132 = CARTESIAN_POINT ( 'NONE',  ( -10.95209178422446605, 15.32973516857846796, -1.791032230336580211 ) ) ;
#20133 = CARTESIAN_POINT ( 'NONE',  ( -0.3063878209169000333, 25.36830905619000021, 2.314903654952999990 ) ) ;
#20134 = CARTESIAN_POINT ( 'NONE',  ( 14.66098616093672469, 6.531434504799800145, -7.997021604459393807 ) ) ;
#20135 = DIRECTION ( 'NONE',  ( 0.000000000000000000, 1.000000000000000000, 0.000000000000000000 ) ) ;
#20136 = CARTESIAN_POINT ( 'NONE',  ( 20.38110275387000314, 11.05129809220999881, 1.830737130756000086 ) ) ;
#20137 = DIRECTION ( 'NONE',  ( 0.000000000000000000, -1.000000000000000000, 0.000000000000000000 ) ) ;
#20138 = CARTESIAN_POINT ( 'NONE',  ( 13.80182517639457274, 9.025292127787466256, 0.004672145026744048760 ) ) ;
#20139 = LINE ( 'NONE', #3547, #10011 ) ;
#20140 = FILL_AREA_STYLE_COLOUR ( '', #18364 ) ;
#20141 = B_SPLINE_CURVE_WITH_KNOTS ( 'NONE', 3,
 ( #7727, #22488, #15335, #20446, #13170, #13283, #22372, #13049, #17162, #2035, #557, #7842, #2507, #7477, #11606, #5897 ),
 .UNSPECIFIED., .F., .F.,
 ( 4, 2, 2, 2, 2, 2, 2, 4 ),
 ( 0.000000000000000000, 0.2500000000000000000, 0.3750000000000000000, 0.4375000000000000000, 0.4687500000000000000, 0.5000000000000000000, 0.7500000000000000000, 1.000000000000000000 ),
 .UNSPECIFIED. ) ;
#20142 = EDGE_LOOP ( 'NONE', ( #1752, #7829, #9763, #17788 ) ) ;
#20143 = CARTESIAN_POINT ( 'NONE',  ( -14.84820223132186356, -7.755096387757968834, -4.693416038378982691 ) ) ;
#20144 = CARTESIAN_POINT ( 'NONE',  ( -2.327192509895188000, 28.00639765414752702, 3.274853329251978362 ) ) ;
#20145 = ORIENTED_EDGE ( 'NONE', *, *, #19656, .T. ) ;
#20146 = CARTESIAN_POINT ( 'NONE',  ( 19.05233531832000082, -1.887707665395999879, 10.26617185442000135 ) ) ;
#20147 = CARTESIAN_POINT ( 'NONE',  ( 1.980818591402529361, 30.73245735271817836, -1.143255368690362150 ) ) ;
#20148 = FACE_OUTER_BOUND ( 'NONE', #13578, .T. ) ;
#20149 = CARTESIAN_POINT ( 'NONE',  ( 24.34804274388871193, 3.330488627411498204, -12.50000000000000355 ) ) ;
#20150 = CARTESIAN_POINT ( 'NONE',  ( -16.45626648132295955, 9.977493378410441593, 2.951365295957959489 ) ) ;
#20151 = CARTESIAN_POINT ( 'NONE',  ( 2.429928970624000151, 27.96256359723999907, 0.4339301335947000626 ) ) ;
#20152 = ORIENTED_EDGE ( 'NONE', *, *, #11324, .F. ) ;
#20153 = CARTESIAN_POINT ( 'NONE',  ( -9.392652565846001167, -11.23270293799999919, -9.740851948633999058 ) ) ;
#20154 = CARTESIAN_POINT ( 'NONE',  ( 13.49999999999999822, 9.583219496692837680, 0.7036459153352878637 ) ) ;
#20155 = CARTESIAN_POINT ( 'NONE',  ( -14.45561352951336964, -12.11761689492659677, -4.011600805616156507 ) ) ;
#20156 = EDGE_CURVE ( 'NONE', #19018, #14183, #4398, .T. ) ;
#20157 = ORIENTED_EDGE ( 'NONE', *, *, #23593, .T. ) ;
#20158 = CARTESIAN_POINT ( 'NONE',  ( 22.94113296525130252, -10.36727481655944771, -2.169730993702538413 ) ) ;
#20159 = CARTESIAN_POINT ( 'NONE',  ( 12.52688711657000020, -13.93375672974000068, 0.8660254037843999608 ) ) ;
#20160 = CARTESIAN_POINT ( 'NONE',  ( 15.97207963789832164, -9.022303258340008014, -5.088742242062048504 ) ) ;
#20161 = FACE_OUTER_BOUND ( 'NONE', #4401, .T. ) ;
#20162 = CARTESIAN_POINT ( 'NONE',  ( 0.5113872014135000255, 30.80268660612999909, -2.127704381286000146 ) ) ;
#20163 = CIRCLE ( 'NONE', #798, 9.287173237303996132 ) ;
#20164 = CARTESIAN_POINT ( 'NONE',  ( -19.04882659540000134, -6.818301851232999589, 6.682161380682999585 ) ) ;
#20165 = ADVANCED_FACE ( 'NONE', ( #1689, #329 ), #2157, .T. ) ;
#20166 = CARTESIAN_POINT ( 'NONE',  ( 2.110692983767971764, 29.83106853030913186, -0.4604840047560345151 ) ) ;
#20167 = VERTEX_POINT ( 'NONE', #99 ) ;
#20168 = CARTESIAN_POINT ( 'NONE',  ( -2.169404915079000240, 24.61931165514999975, -0.2292880595415000000 ) ) ;
#20169 = CARTESIAN_POINT ( 'NONE',  ( 19.87364837678908813, -1.149180406892156281, -10.44631844158005407 ) ) ;
#20170 = LINE ( 'NONE', #10959, #23838 ) ;
#20171 = VERTEX_POINT ( 'NONE', #7484 ) ;
#20172 = CARTESIAN_POINT ( 'NONE',  ( 4.851389421338315522, 14.56759478981999933, -3.780608026316847337 ) ) ;
#20173 = CARTESIAN_POINT ( 'NONE',  ( -4.197096011533001381, 12.18682765224999187, -2.415895191620001992 ) ) ;
#20174 = ORIENTED_EDGE ( 'NONE', *, *, #2998, .T. ) ;
#20175 = CARTESIAN_POINT ( 'NONE',  ( 17.75418875731000057, 8.769310764750999354, 2.911614084577999861 ) ) ;
#20176 = ORIENTED_EDGE ( 'NONE', *, *, #7863, .F. ) ;
#20177 = CARTESIAN_POINT ( 'NONE',  ( 2.504532394112000003E-14, 28.43419673618999965, 2.500000000000000000 ) ) ;
#20178 = APPLICATION_PROTOCOL_DEFINITION ( 'draft international standard', 'automotive_design', 1998, #22110 ) ;
#20179 = CARTESIAN_POINT ( 'NONE',  ( 18.51344355829000321, -13.93375672974000068, 0.000000000000000000 ) ) ;
#20180 = EDGE_CURVE ( 'NONE', #5053, #19500, #7734, .T. ) ;
#20181 = ORIENTED_EDGE ( 'NONE', *, *, #4322, .F. ) ;
#20182 = CARTESIAN_POINT ( 'NONE',  ( 2.500000000000000000, 24.40000000000000213, 0.000000000000000000 ) ) ;
#20183 = CARTESIAN_POINT ( 'NONE',  ( -22.24049188378000252, 9.221077711103999874, 5.343197927521000423 ) ) ;
#20184 = CARTESIAN_POINT ( 'NONE',  ( -17.38633714188999946, 9.179352961803999733, 3.390708539619000206 ) ) ;
#20185 = CARTESIAN_POINT ( 'NONE',  ( -5.123170459737996119, 14.39942909848998909, -4.079011992021998267 ) ) ;
#20186 = CARTESIAN_POINT ( 'NONE',  ( -22.44018545090364469, 6.612455538562568513, -8.384770958092557791 ) ) ;
#20187 = CARTESIAN_POINT ( 'NONE',  ( -1.712953330202006796, 27.71795734230703445, -1.393201056469692611 ) ) ;
#20188 = PLANE ( 'NONE',  #22032 ) ;
#20189 = EDGE_CURVE ( 'NONE', #2380, #1933, #4889, .T. ) ;
#20190 = CARTESIAN_POINT ( 'NONE',  ( 1.602509900017840216, 30.69733188989498274, -1.449043562559991338 ) ) ;
#20191 = ORIENTED_EDGE ( 'NONE', *, *, #6382, .T. ) ;
#20192 = CARTESIAN_POINT ( 'NONE',  ( 23.96715810487390286, -8.818041421502185173, 3.119150737227263992 ) ) ;
#20193 = DIRECTION ( 'NONE',  ( 0.9996708941621511579, 0.02565352539213875543, 0.000000000000000000 ) ) ;
#20194 = CARTESIAN_POINT ( 'NONE',  ( 14.30901013702234081, 6.517998721482895164, 6.337184079108406642 ) ) ;
#20195 = CIRCLE ( 'NONE', #2390, 12.50000000000000178 ) ;
#20196 = DIRECTION ( 'NONE',  ( -1.000000000000000000, 0.000000000000000000, 0.000000000000000000 ) ) ;
#20197 = CARTESIAN_POINT ( 'NONE',  ( 0.4700916780637000580, 28.86021896306000301, 2.089231778180999921 ) ) ;
#20198 = CARTESIAN_POINT ( 'NONE',  ( -14.25243324638999809, -13.93375672974000068, -0.8660254037843999608 ) ) ;
#20199 = CARTESIAN_POINT ( 'NONE',  ( 2.248627110350167158, 11.69740771678675451, 4.262999372637977125 ) ) ;
#20200 = ORIENTED_EDGE ( 'NONE', *, *, #7490, .T. ) ;
#20201 = ADVANCED_FACE ( 'NONE', ( #10905 ), #7575, .F. ) ;
#20202 = CARTESIAN_POINT ( 'NONE',  ( -1.562092572808364777, 11.58646502489367869, -4.556008495004664205 ) ) ;
#20203 = CARTESIAN_POINT ( 'NONE',  ( 3.653528746108709147, 28.20780860099632648, 2.509315635922550580 ) ) ;
#20204 = CARTESIAN_POINT ( 'NONE',  ( 2.220102258368206183, 28.80150489129345814, 0.5102462943910046622 ) ) ;
#20205 = ORIENTED_EDGE ( 'NONE', *, *, #11327, .F. ) ;
#20206 = EDGE_CURVE ( 'NONE', #13196, #3402, #23840, .T. ) ;
#20207 = SHAPE_REPRESENTATION ( 'Rotary Valve Ball', ( #4390 ), #17940 ) ;
#20208 = EDGE_CURVE ( 'NONE', #19206, #2201, #18261, .T. ) ;
#20209 = DIRECTION ( 'NONE',  ( 0.000000000000000000, -1.000000000000000000, 0.000000000000000000 ) ) ;
#20210 = CARTESIAN_POINT ( 'NONE',  ( -16.40405420454666086, -1.190044756772769441, -9.092242074617137959 ) ) ;
#20211 = CARTESIAN_POINT ( 'NONE',  ( 16.60050158530999909, 6.318772076511000257, 8.042630855556000213 ) ) ;
#20212 = CARTESIAN_POINT ( 'NONE',  ( 18.54963726174204552, 10.44196517788747336, 0.1308933847890557112 ) ) ;
#20213 = CARTESIAN_POINT ( 'NONE',  ( 12.52688711657000020, 6.216878364870000340, 12.50000000000000000 ) ) ;
#20214 = CARTESIAN_POINT ( 'NONE',  ( 1.778641839820999992, 29.13930575949000001, -1.523279337374999987 ) ) ;
#20215 = CARTESIAN_POINT ( 'NONE',  ( -12.50492312419000207, 6.877612380107000156, -5.798846373018999856 ) ) ;
#20216 = CARTESIAN_POINT ( 'NONE',  ( 13.50000000000000355, -9.024405030093623381, -2.976340912779337433 ) ) ;
#20217 = CIRCLE ( 'NONE', #2021, 12.50000000000000000 ) ;
#20218 = EDGE_LOOP ( 'NONE', ( #2101, #7807, #12267 ) ) ;
#20219 = CARTESIAN_POINT ( 'NONE',  ( -24.46742986864630964, 11.46616815105915244, 5.140026613611447637 ) ) ;
#20220 = CARTESIAN_POINT ( 'NONE',  ( 19.23935571152999913, -9.634227767086001037, 5.773988190026000389 ) ) ;
#20221 = EDGE_CURVE ( 'NONE', #8499, #10321, #10763, .T. ) ;
#20222 = CARTESIAN_POINT ( 'NONE',  ( -14.25699038479000080, 13.93375672974000068, 0.000000000000000000 ) ) ;
#20223 = EDGE_CURVE ( 'NONE', #6590, #17924, #17241, .T. ) ;
#20224 = DIRECTION ( 'NONE',  ( 0.5000000000000169864, 0.000000000000000000, -0.8660254037844289376 ) ) ;
#20225 = CARTESIAN_POINT ( 'NONE',  ( 24.50000000000000000, -1.624284714732273649, 10.43931695975270202 ) ) ;
#20226 = DIRECTION ( 'NONE',  ( 0.000000000000000000, -1.000000000000000000, 0.000000000000000000 ) ) ;
#20227 = CARTESIAN_POINT ( 'NONE',  ( 0.3048288769163433609, 29.18568722789423475, -2.138368886124048629 ) ) ;
#20228 = CARTESIAN_POINT ( 'NONE',  ( -22.31075685788999863, 0.1502046266062000146, -11.11246732393999892 ) ) ;
#20229 = ORIENTED_EDGE ( 'NONE', *, *, #2904, .T. ) ;
#20230 = CARTESIAN_POINT ( 'NONE',  ( 1.940453181907765057, 23.84595057970013343, 1.348463719542498440 ) ) ;
#20231 = ORIENTED_EDGE ( 'NONE', *, *, #7592, .T. ) ;
#20232 = CARTESIAN_POINT ( 'NONE',  ( 1.940602815664000058, 25.78657252654999965, -0.6793350042104999709 ) ) ;
#20233 = CARTESIAN_POINT ( 'NONE',  ( 0.000000000000000000, 24.65000000000000213, 0.000000000000000000 ) ) ;
#20234 = CYLINDRICAL_SURFACE ( 'NONE', #3401, 2.000000000000000000 ) ;
#20235 = VECTOR ( 'NONE', #15756, 1000.000000000000000 ) ;
#20236 = CARTESIAN_POINT ( 'NONE',  ( -16.81976253787999909, -9.102909969768001375, 0.000000000000000000 ) ) ;
#20237 = DIRECTION ( 'NONE',  ( 0.000000000000000000, 1.000000000000000000, 0.000000000000000000 ) ) ;
#20238 = CARTESIAN_POINT ( 'NONE',  ( 16.27143908530999639, 9.938600131338999333, -2.378686727414999869 ) ) ;
#20239 =( LENGTH_UNIT ( ) NAMED_UNIT ( * ) SI_UNIT ( .MILLI., .METRE. ) );
#20240 = ORIENTED_EDGE ( 'NONE', *, *, #20221, .T. ) ;
#20241 = CARTESIAN_POINT ( 'NONE',  ( -13.72667946694999941, 4.336095440212999641, 8.658528082053999597 ) ) ;
#20242 = DIRECTION ( 'NONE',  ( -1.000000000000000000, 0.000000000000000000, 0.000000000000000000 ) ) ;
#20243 = CARTESIAN_POINT ( 'NONE',  ( 10.35615758860000035, 0.000000000000000000, 0.000000000000000000 ) ) ;
#20244 = ORIENTED_EDGE ( 'NONE', *, *, #9614, .F. ) ;
#20245 = CARTESIAN_POINT ( 'NONE',  ( -19.82024391687000175, 2.079266777114999964, 10.99594615337999848 ) ) ;
#20246 = CARTESIAN_POINT ( 'NONE',  ( 2.132304841933000183, 25.62447351380000171, -0.6819187252057000714 ) ) ;
#20247 = CARTESIAN_POINT ( 'NONE',  ( 14.86624431231352439, 10.19680779959737471, -1.809567902645908166 ) ) ;
#20248 = CARTESIAN_POINT ( 'NONE',  ( -17.99130420454667245, 5.612729004169484170, -7.303246745062192957 ) ) ;
#20249 = CARTESIAN_POINT ( 'NONE',  ( 24.38221057305000272, 6.592218218594999790, 9.192201995134999137 ) ) ;
#20250 = CARTESIAN_POINT ( 'NONE',  ( 1.526121187041999949, 28.78992591556999869, 1.539885762186999907 ) ) ;
#20251 = EDGE_CURVE ( 'NONE', #21708, #17770, #18030, .T. ) ;
#20252 = CARTESIAN_POINT ( 'NONE',  ( 14.05462922766051648, 5.715449972624886854, 7.003620237176114038 ) ) ;
#20253 = CARTESIAN_POINT ( 'NONE',  ( -4.159224151219002685, 12.40416002829998732, -2.437210981237998730 ) ) ;
#20254 =( GEOMETRIC_REPRESENTATION_CONTEXT ( 3 ) GLOBAL_UNCERTAINTY_ASSIGNED_CONTEXT ( ( #1677 ) ) GLOBAL_UNIT_ASSIGNED_CONTEXT ( ( #20239, #7384, #16588 ) ) REPRESENTATION_CONTEXT ( 'NONE', 'WORKASPACE' ) );
#20255 = CARTESIAN_POINT ( 'NONE',  ( -22.22397087121331438, -9.241592606737556892, -1.209848591021944531 ) ) ;
#20256 = ORIENTED_EDGE ( 'NONE', *, *, #11562, .F. ) ;
#20257 = CARTESIAN_POINT ( 'NONE',  ( -14.55352821834695298, 0.01803078645220980436, -9.054618933368537625 ) ) ;
#20258 = CARTESIAN_POINT ( 'NONE',  ( -14.11574458423267586, -9.891920035128775268, 3.515509136289259207 ) ) ;
#20259 = CIRCLE ( 'NONE', #12137, 0.09999993872260067029 ) ;
#20260 = ORIENTED_EDGE ( 'NONE', *, *, #5527, .F. ) ;
#20261 = CARTESIAN_POINT ( 'NONE',  ( -16.37216243917331582, -7.943913672023831474, -4.578730802673559808 ) ) ;
#20262 = DIRECTION ( 'NONE',  ( 0.000000000000000000, 1.000000000000000000, 0.000000000000000000 ) ) ;
#20263 = CARTESIAN_POINT ( 'NONE',  ( -23.50032910583999879, 3.801543240379000377, -8.459419100777001432 ) ) ;
#20264 = CARTESIAN_POINT ( 'NONE',  ( 15.02018438422999935, 6.390136118733999560, 8.990257899662001506 ) ) ;
#20265 = DIRECTION ( 'NONE',  ( -0.7071067811865975328, 0.7071067811864976127, 1.204882835872995245E-09 ) ) ;
#20266 = CARTESIAN_POINT ( 'NONE',  ( 0.6153010951426000075, 27.94669433610000198, -2.804372049896000085 ) ) ;
#20267 = VERTEX_POINT ( 'NONE', #16192 ) ;
#20268 = CARTESIAN_POINT ( 'NONE',  ( -9.799942565846000875, -8.137225276125999329, 12.44360880412000014 ) ) ;
#20269 = B_SPLINE_CURVE_WITH_KNOTS ( 'NONE', 3,
 ( #11859, #8113, #8472, #22864, #8591 ),
 .UNSPECIFIED., .F., .F.,
 ( 4, 1, 4 ),
 ( 0.000000000000000000, 0.5000000000000000000, 1.000000000000000000 ),
 .UNSPECIFIED. ) ;
#20270 = DIRECTION ( 'NONE',  ( -1.000000000000000000, 5.341664343519000084E-12, -4.885518282254999468E-11 ) ) ;
#20271 = CARTESIAN_POINT ( 'NONE',  ( 4.649999849441000421, 22.00000015055399771, -6.648422772555000414E-08 ) ) ;
#20272 = ORIENTED_EDGE ( 'NONE', *, *, #9193, .F. ) ;
#20273 = CARTESIAN_POINT ( 'NONE',  ( 20.85099770046331358, -1.205236576247627367, -9.206359409188111798 ) ) ;
#20274 = CARTESIAN_POINT ( 'NONE',  ( 24.15736593521593178, 8.253730364077119575, -10.70411965744399119 ) ) ;
#20275 = CARTESIAN_POINT ( 'NONE',  ( 16.18754222806948562, -3.151203986297408388, -9.872908633960614466 ) ) ;
#20276 = CARTESIAN_POINT ( 'NONE',  ( -19.13544413845999870, -9.637273350829000051, -5.571910801056999318 ) ) ;
#20277 = FACE_OUTER_BOUND ( 'NONE', #13238, .T. ) ;
#20278 = AXIS2_PLACEMENT_3D ( 'NONE', #19247, #10053, #8118 ) ;
#20279 = CARTESIAN_POINT ( 'NONE',  ( -16.81439276773000202, -8.006006257143999605, -6.488443847660000152 ) ) ;
#20280 = CARTESIAN_POINT ( 'NONE',  ( 1.352523426442719501, 29.91753472705243766, -1.683999728453754674 ) ) ;
#20281 = VERTEX_POINT ( 'NONE', #8702 ) ;
#20282 = CARTESIAN_POINT ( 'NONE',  ( 1.961934450082000181, 25.63159458490000020, -0.6881597550252999129 ) ) ;
#20283 = CARTESIAN_POINT ( 'NONE',  ( 20.12900882975453243, 7.359272468721639093, -7.512247993263142298 ) ) ;
#20284 = CYLINDRICAL_SURFACE ( 'NONE', #20001, 10.59999999999999964 ) ;
#20285 = ORIENTED_EDGE ( 'NONE', *, *, #19614, .T. ) ;
#20286 = EDGE_CURVE ( 'NONE', #17545, #20307, #18803, .T. ) ;
#20287 = CARTESIAN_POINT ( 'NONE',  ( 4.860820541961833996, 14.52075968249973670, -3.787349904231070763 ) ) ;
#20288 = CARTESIAN_POINT ( 'NONE',  ( -4.832579888156002035, 12.42138610322999526, -0.3261195631766998226 ) ) ;
#20289 = EDGE_LOOP ( 'NONE', ( #9143, #19382, #23698, #4754 ) ) ;
#20290 = CARTESIAN_POINT ( 'NONE',  ( 12.16012625731000085, 8.900490462747001175, -1.861105101465000189 ) ) ;
#20291 = ORIENTED_EDGE ( 'NONE', *, *, #14578, .F. ) ;
#20292 = CARTESIAN_POINT ( 'NONE',  ( -3.776477861809037329, 14.59612568772429952, 4.825021002418410809 ) ) ;
#20293 = PRODUCT_CONTEXT ( 'NONE', #11751, 'mechanical' ) ;
#20294 = CARTESIAN_POINT ( 'NONE',  ( -14.49284521823309824, 1.036537809063993176, -12.49997544920737802 ) ) ;
#20295 = ADVANCED_FACE ( 'NONE', ( #15802 ), #20721, .F. ) ;
#20296 = ORIENTED_EDGE ( 'NONE', *, *, #20786, .F. ) ;
#20297 = CARTESIAN_POINT ( 'NONE',  ( 2.184730091557438136, 24.46663824537979082, -1.258552818647198146 ) ) ;
#20298 = AXIS2_PLACEMENT_3D ( 'NONE', #16119, #3311, #15879 ) ;
#20299 = CARTESIAN_POINT ( 'NONE',  ( 12.00000000000000178, 3.061724608921426949, -8.619331017259337813 ) ) ;
#20300 = CARTESIAN_POINT ( 'NONE',  ( -19.82390131753000162, -2.296328123436000457, -9.582100204323001691 ) ) ;
#20301 = CARTESIAN_POINT ( 'NONE',  ( 18.48816666666665398, -7.991458167462555551, -4.605843167114078263 ) ) ;
#20302 = CARTESIAN_POINT ( 'NONE',  ( -22.92915284010549470, -9.027613226242038991, -5.491954109625697633 ) ) ;
#20303 = CARTESIAN_POINT ( 'NONE',  ( 11.01624327026000039, -12.44999999999999929, 0.000000000000000000 ) ) ;
#20304 = CARTESIAN_POINT ( 'NONE',  ( 15.80495833333332634, 7.258560212986407301, 5.578069749145255329 ) ) ;
#20305 = CARTESIAN_POINT ( 'NONE',  ( -5.983850654344998077, 15.83682997010998506, 0.8930707396852997082 ) ) ;
#20306 = CARTESIAN_POINT ( 'NONE',  ( 1.967353437452023623, 30.65813742271244635, -0.8921482303055430219 ) ) ;
#20307 = VERTEX_POINT ( 'NONE', #19203 ) ;
#20308 = CYLINDRICAL_SURFACE ( 'NONE', #20828, 2.750000000000000000 ) ;
#20309 = CARTESIAN_POINT ( 'NONE',  ( 4.495985175916063170, 13.47622785279660462, -5.169691691112981324 ) ) ;
#20310 = EDGE_CURVE ( 'NONE', #5650, #367, #22571, .T. ) ;
#20311 = CARTESIAN_POINT ( 'NONE',  ( -23.02737179241879772, -9.363639631091235316, 4.904215814585074718 ) ) ;
#20312 = CARTESIAN_POINT ( 'NONE',  ( -0.3134588398365999451, 28.01521896306000059, 2.266239109532000029 ) ) ;
#20313 = CARTESIAN_POINT ( 'NONE',  ( 0.000000000000000000, 8.900000000000000355, 0.000000000000000000 ) ) ;
#20314 = ORIENTED_EDGE ( 'NONE', *, *, #19989, .F. ) ;
#20315 = CARTESIAN_POINT ( 'NONE',  ( -4.637553514248847542, 12.37005176196437262, -1.410038579757167509 ) ) ;
#20316 = CARTESIAN_POINT ( 'NONE',  ( 24.00034722001000276, -7.216970193686000457, -11.92259671342000082 ) ) ;
#20317 = CARTESIAN_POINT ( 'NONE',  ( -1.009755838453245902, 29.08874043368814810, -2.041968248507524564 ) ) ;
#20318 = ORIENTED_EDGE ( 'NONE', *, *, #2254, .T. ) ;
#20319 = EDGE_CURVE ( 'NONE', #9272, #2748, #18041, .T. ) ;
#20320 = CARTESIAN_POINT ( 'NONE',  ( 4.000000000000000000, 26.20000000000000284, 2.309401076759000304 ) ) ;
#20321 = CARTESIAN_POINT ( 'NONE',  ( 14.62612658531000243, 9.561303730670999812, 3.483288127948000135 ) ) ;
#20322 = CARTESIAN_POINT ( 'NONE',  ( 17.80562055465178517, -8.706723506620447139, -5.795109365428579906 ) ) ;
#20323 = CARTESIAN_POINT ( 'NONE',  ( 21.45754691133435799, 36.29044427405532502, 6.000000000000005329 ) ) ;
#20324 = CARTESIAN_POINT ( 'NONE',  ( 0.9055761032497999796, 30.68836414079000008, -1.950832896806000027 ) ) ;
#20325 = LINE ( 'NONE', #1576, #12040 ) ;
#20326 = CARTESIAN_POINT ( 'NONE',  ( 13.49999999999999645, -8.571874797152489123, 5.143046839193468500 ) ) ;
#20327 = AXIS2_PLACEMENT_3D ( 'NONE', #10898, #14749, #3861 ) ;
#20328 = VERTEX_POINT ( 'NONE', #23679 ) ;
#20329 = EDGE_CURVE ( 'NONE', #9720, #1224, #16161, .T. ) ;
#20330 = DIRECTION ( 'NONE',  ( 0.000000000000000000, -1.000000000000000000, 0.000000000000000000 ) ) ;
#20331 = CARTESIAN_POINT ( 'NONE',  ( 19.06230660937999843, -4.552702152812999614, 10.26188179881000018 ) ) ;
#20332 = CARTESIAN_POINT ( 'NONE',  ( -24.50000000000000000, 3.293267271483000247, -9.759323269498999309 ) ) ;
#20333 = ORIENTED_EDGE ( 'NONE', *, *, #18883, .T. ) ;
#20334 = DIRECTION ( 'NONE',  ( 0.000000000000000000, 1.000000000000000000, 0.000000000000000000 ) ) ;
#20335 = CARTESIAN_POINT ( 'NONE',  ( 18.75008227645999881, 0.000000000000000000, 0.000000000000000000 ) ) ;
#20336 = CARTESIAN_POINT ( 'NONE',  ( 4.023773140947001004, 12.12796709211999513, 2.696238718279999169 ) ) ;
#20337 = CARTESIAN_POINT ( 'NONE',  ( -0.7609346232008592503, 29.24959062363414475, -2.021388052729749418 ) ) ;
#20338 = ADVANCED_FACE ( 'NONE', ( #18124 ), #1286, .F. ) ;
#20339 = CARTESIAN_POINT ( 'NONE',  ( 12.51793260380000028, 13.93375672974000068, -0.7216754077441999149 ) ) ;
#20340 = VERTEX_POINT ( 'NONE', #4925 ) ;
#20341 = CARTESIAN_POINT ( 'NONE',  ( -7.034000000000000696, 10.69999999999999929, -6.692428833332999144E-10 ) ) ;
#20342 = VERTEX_POINT ( 'NONE', #6972 ) ;
#20343 = CARTESIAN_POINT ( 'NONE',  ( -0.04029237313626999467, 24.84695296423999977, 2.352876976275999787 ) ) ;
#20344 =( BOUNDED_SURFACE ( )  B_SPLINE_SURFACE ( 3, 3, ( 
 ( #15384, #15506, #4267, #21088, #20855, #6190, #19025, #2437 ),
 ( #23013, #13576, #2555, #9945, #8140, #6430, #13815, #21214 ),
 ( #4629, #2813, #8379, #12497, #3180, #8981, #14064, #17834 ),
 ( #5116, #8621, #16353, #15982, #18302, #14188, #21458, #9092 ) ),
 .UNSPECIFIED., .F., .F., .T. ) 
 B_SPLINE_SURFACE_WITH_KNOTS ( ( 4, 4 ),
 ( 4, 1, 1, 1, 1, 4 ),
 ( 0.000000000000000000, 1.000000000000000000 ),
 ( 0.005250863527401000187, 0.01452849757938999911, 0.02864204905892000011, 0.04333368315689999778, 0.05817056875622000217, 0.06131925226894999886 ),
 .UNSPECIFIED. ) 
 GEOMETRIC_REPRESENTATION_ITEM ( )  RATIONAL_B_SPLINE_SURFACE ( (
 ( 1.226455171705000069, 1.226455171705000069, 1.226455171705000069, 1.226455171705000069, 1.226455171705000069, 1.226455171705000069, 1.226455171705000069, 1.226455171705000069),
 ( 0.9245149427651999652, 0.9245149427651999652, 0.9245149427651999652, 0.9245149427651999652, 0.9245149427651999652, 0.9245149427651999652, 0.9245149427651999652, 0.9245149427651999652),
 ( 0.9245149427651999652, 0.9245149427651999652, 0.9245149427651999652, 0.9245149427651999652, 0.9245149427651999652, 0.9245149427651999652, 0.9245149427651999652, 0.9245149427651999652),
 ( 1.226455171705000069, 1.226455171705000069, 1.226455171705000069, 1.226455171705000069, 1.226455171705000069, 1.226455171705000069, 1.226455171705000069, 1.226455171705000069) ) ) 
 REPRESENTATION_ITEM ( '' )  SURFACE ( )  );
#20345 = CARTESIAN_POINT ( 'NONE',  ( 5.991097115754002722, 13.66124479386999546, 2.878337485509001592 ) ) ;
#20346 = CIRCLE ( 'NONE', #21102, 3.000000000000000000 ) ;
#20347 = CARTESIAN_POINT ( 'NONE',  ( 5.506614905180002850, 13.75449879388000518, 4.409302736622996655 ) ) ;
#20348 = AXIS2_PLACEMENT_3D ( 'NONE', #9144, #22564, #18588 ) ;
#20349 = DIRECTION ( 'NONE',  ( 0.5000000000000169864, 0.000000000000000000, -0.8660254037844289376 ) ) ;
#20350 = DIRECTION ( 'NONE',  ( 0.000000000000000000, 1.000000000000000000, 0.000000000000000000 ) ) ;
#20351 = CARTESIAN_POINT ( 'NONE',  ( 17.50443924930999984, -10.75095007791999890, -0.4607405056646999841 ) ) ;
#20352 = ADVANCED_FACE ( 'NONE', ( #5166 ), #19701, .T. ) ;
#20353 = VERTEX_POINT ( 'NONE', #19935 ) ;
#20354 = CARTESIAN_POINT ( 'NONE',  ( -13.52354911898000012, -2.293961044660999704, 9.402123702338000655 ) ) ;
#20355 = DIRECTION ( 'NONE',  ( -1.000000000000000000, 0.000000000000000000, 0.000000000000000000 ) ) ;
#20356 = CARTESIAN_POINT ( 'NONE',  ( 0.000000000000000000, -1.550000000000000044, 0.000000000000000000 ) ) ;
#20357 = EDGE_LOOP ( 'NONE', ( #20157, #19663, #4018, #14059 ) ) ;
#20358 = CARTESIAN_POINT ( 'NONE',  ( -10.60269991523250610, 15.46630580253647835, -1.465288580574494404 ) ) ;
#20359 = CARTESIAN_POINT ( 'NONE',  ( -0.8815400351514000032, 24.53577456897999909, 2.162298408882000089 ) ) ;
#20360 = CARTESIAN_POINT ( 'NONE',  ( 14.54356512408170587, 2.819943630748654506, -9.929365919741389490 ) ) ;
#20361 = CARTESIAN_POINT ( 'NONE',  ( 60.61494135913342518, 37.01856778792605240, -2.673746900119611247 ) ) ;
#20362 = CARTESIAN_POINT ( 'NONE',  ( 22.73028790635000007, 0.6840553180648999421, 11.24560851965999930 ) ) ;
#20363 = CARTESIAN_POINT ( 'NONE',  ( -1.942407726809000090, 30.58970545120000040, -1.656974607114999998 ) ) ;
#20364 = CARTESIAN_POINT ( 'NONE',  ( 13.80157322160490629, 9.025297321909626191, -0.003338010211690475675 ) ) ;
#20365 = CARTESIAN_POINT ( 'NONE',  ( -6.319385089483436246, 15.63721120038809609, -1.258692299061803466 ) ) ;
#20366 = AXIS2_PLACEMENT_3D ( 'NONE', #21609, #23532, #5026 ) ;
#20367 = CIRCLE ( 'NONE', #16483, 3.000000000000000000 ) ;
#20368 = LINE ( 'NONE', #13319, #18532 ) ;
#20369 = ADVANCED_FACE ( 'NONE', ( #16039 ), #16462, .T. ) ;
#20370 = CARTESIAN_POINT ( 'NONE',  ( 12.12543434882655902, 13.45291906885516298, -1.698934468806289733 ) ) ;
#20371 = ORIENTED_EDGE ( 'NONE', *, *, #2278, .F. ) ;
#20372 = B_SPLINE_CURVE_WITH_KNOTS ( 'NONE', 3,
 ( #6751, #12096, #12213, #15582, #6512, #13896, #12337, #14144, #21298, #19227, #2890, #23216, #4582, #14022, #19729, #10270, #17538, #13768, #15941, #933, #19361, #3140, #10152, #10524, #17907, #16064, #23460, #4711, #8699, #8331, #21170, #17661, #11973, #6873, #21045, #4457, #1058, #19603, #11848, #2767, #8459, #6632, #21413, #3011, #10398, #17790, #1188, #12691, #12458, #18488, #16543, #16189, #23812, #1556, #10640, #5422, #22008, #1432, #23935, #18369, #23590, #10984, #21890 ),
 .UNSPECIFIED., .F., .F.,
 ( 4, 2, 2, 1, 1, 1, 1, 1, 2, 2, 2, 2, 1, 1, 1, 1, 2, 2, 2, 1, 1, 1, 2, 2, 2, 2, 1, 1, 1, 1, 2, 2, 2, 2, 1, 1, 1, 2, 2, 2, 4 ),
 ( 0.000000000000000000, 0.1249999999999909239, 0.1874999999999864830, 0.2187499999999842903, 0.2343749999999831524, 0.2421874999999825140, 0.2460937499999820144, 0.2480468749999818479, 0.2490234374999818479, 0.2499999999999818201, 0.3749999999999766298, 0.4374999999999740763, 0.4687499999999727440, 0.4843749999999720224, 0.4921874999999716893, 0.4960937499999715228, 0.4980468749999714673, 0.4999999999999713562, 0.5624999999999680256, 0.5937499999999663602, 0.6093749999999654721, 0.6171874999999651390, 0.6210937499999650280, 0.6249999999999648059, 0.6874999999999620304, 0.7187499999999605871, 0.7343749999999598099, 0.7421874999999594769, 0.7460937499999591438, 0.7480468749999590328, 0.7490234374999588107, 0.7499999999999585887, 0.8124999999999679146, 0.8437499999999724665, 0.8593749999999746869, 0.8671874999999759082, 0.8710937499999764633, 0.8730468749999767963, 0.8749999999999771294, 0.9374999999999885647, 1.000000000000000000 ),
 .UNSPECIFIED. ) ;
#20373 = EDGE_CURVE ( 'NONE', #1761, #15263, #2547, .T. ) ;
#20374 = CARTESIAN_POINT ( 'NONE',  ( 1.678813317411953054, 30.00000000000000355, -3.649538832790644616 ) ) ;
#20375 = ORIENTED_EDGE ( 'NONE', *, *, #10462, .T. ) ;
#20376 = CARTESIAN_POINT ( 'NONE',  ( -4.000000000000000000, 28.30000000000000071, -2.309401076759000304 ) ) ;
#20377 = DIRECTION ( 'NONE',  ( -0.9996708941621513800, 0.02565352539213145919, 0.000000000000000000 ) ) ;
#20378 = CARTESIAN_POINT ( 'NONE',  ( 12.00000000000000355, 4.044007772105016940, -8.050681685784468300 ) ) ;
#20379 = CIRCLE ( 'NONE', #9925, 4.000000000000000000 ) ;
#20380 = CARTESIAN_POINT ( 'NONE',  ( 17.65928924998999960, -10.44232512227000065, 3.770426973323999675 ) ) ;
#20381 = CARTESIAN_POINT ( 'NONE',  ( -23.75395899076999839, -6.467918998394999619, 12.35506162266000096 ) ) ;
#20382 = CARTESIAN_POINT ( 'NONE',  ( 0.4693273880718999980, 26.10212896667000138, 2.628147087956000050 ) ) ;
#20383 = ADVANCED_FACE ( 'NONE', ( #3116 ), #15918, .F. ) ;
#20384 = ORIENTED_EDGE ( 'NONE', *, *, #21326, .T. ) ;
#20385 = B_SPLINE_CURVE_WITH_KNOTS ( 'NONE', 3,
 ( #8145, #4756, #2442, #11777, #2561, #9833, #13581, #2818, #9951, #10198 ),
 .UNSPECIFIED., .F., .F.,
 ( 4, 1, 1, 2, 2, 4 ),
 ( 0.000000000000000000, 0.2499999999999996669, 0.3749999999999997224, 0.4374999999999996114, 0.4999999999999995559, 1.000000000000000000 ),
 .UNSPECIFIED. ) ;
#20386 = CIRCLE ( 'NONE', #20756, 7.000000000000000000 ) ;
#20387 = CARTESIAN_POINT ( 'NONE',  ( -10.41087756584999902, 13.64079441408000015, -5.914944034101999648 ) ) ;
#20388 = DIRECTION ( 'NONE',  ( -0.5000000000000169864, 0.000000000000000000, -0.8660254037844289376 ) ) ;
#20389 = CARTESIAN_POINT ( 'NONE',  ( 0.000000000000000000, 0.000000000000000000, 0.000000000000000000 ) ) ;
#20390 = ORIENTED_EDGE ( 'NONE', *, *, #13203, .T. ) ;
#20391 = CARTESIAN_POINT ( 'NONE',  ( -14.25243324638999809, 13.93375672974000068, 0.8660254037843999608 ) ) ;
#20392 = CARTESIAN_POINT ( 'NONE',  ( 20.43528936713000377, -9.195691514035999603, 0.000000000000000000 ) ) ;
#20393 = CARTESIAN_POINT ( 'NONE',  ( 6.243178309830739181, 13.63940964843087578, 1.910546506728590499 ) ) ;
#20394 = CARTESIAN_POINT ( 'NONE',  ( 16.01370422644536262, -8.164120605562965594, -6.375661808576880141 ) ) ;
#20395 = CARTESIAN_POINT ( 'NONE',  ( -14.11091303572000122, -1.546633701460999877, 10.88482645332999965 ) ) ;
#20396 = CARTESIAN_POINT ( 'NONE',  ( -0.7084080111906999599, 28.54437317801999896, 1.954714486706000010 ) ) ;
#20397 = VECTOR ( 'NONE', #6882, 1000.000000000000000 ) ;
#20398 = CARTESIAN_POINT ( 'NONE',  ( -4.000000000000000000, 28.00000000000000000, 0.000000000000000000 ) ) ;
#20399 = CARTESIAN_POINT ( 'NONE',  ( 0.9753730088590640834, 29.66360326960658611, 1.927051000882559428 ) ) ;
#20400 = EDGE_LOOP ( 'NONE', ( #9356, #5750, #6029 ) ) ;
#20401 = CARTESIAN_POINT ( 'NONE',  ( -1.194990091485000017, 24.75890718615000097, 1.825072431729000133 ) ) ;
#20402 = CARTESIAN_POINT ( 'NONE',  ( 21.83141184951952596, 4.028956422608725774, -9.926641748303772772 ) ) ;
#20403 = CARTESIAN_POINT ( 'NONE',  ( -0.8858200100745838856, 23.63223437853404363, -1.939564297548260985 ) ) ;
#20404 = B_SPLINE_CURVE_WITH_KNOTS ( 'NONE', 3,
 ( #4796, #12180, #18917, #9832, #5948, #22543, #20860, #6195, #4271, #13700 ),
 .UNSPECIFIED., .F., .F.,
 ( 4, 2, 2, 2, 4 ),
 ( 0.000000000000000000, 0.1249999999999998335, 0.2499999999999996669, 0.4999999999999996669, 1.000000000000000000 ),
 .UNSPECIFIED. ) ;
#20405 = EDGE_LOOP ( 'NONE', ( #16972, #13445 ) ) ;
#20406 = CONICAL_SURFACE ( 'NONE', #21178, 13.97499999999999964, 1.402900403544236729 ) ;
#20407 = CARTESIAN_POINT ( 'NONE',  ( 2.500000000000000000, 30.23419673619000037, 0.000000000000000000 ) ) ;
#20408 = CARTESIAN_POINT ( 'NONE',  ( -23.75856372112281178, -13.93375672973999890, -3.388131789017201356E-17 ) ) ;
#20409 = CARTESIAN_POINT ( 'NONE',  ( 18.32906392130999862, 1.076221949391999999, 9.704785274157000430 ) ) ;
#20410 = ORIENTED_EDGE ( 'NONE', *, *, #18408, .T. ) ;
#20411 = VECTOR ( 'NONE', #19617, 1000.000000000000000 ) ;
#20412 = CARTESIAN_POINT ( 'NONE',  ( -1.259047450927231804, 28.36753006952333322, 2.184465970885654862 ) ) ;
#20413 = DIRECTION ( 'NONE',  ( 0.000000000000000000, 0.000000000000000000, -1.000000000000000000 ) ) ;
#20414 = ORIENTED_EDGE ( 'NONE', *, *, #7789, .T. ) ;
#20415 = CARTESIAN_POINT ( 'NONE',  ( -15.53484587121333504, 2.373919399437545152, 8.833918887178354495 ) ) ;
#20416 = CARTESIAN_POINT ( 'NONE',  ( 4.619606713675000087, 12.56765075308000768, 1.087864528862000579 ) ) ;
#20417 = CARTESIAN_POINT ( 'NONE',  ( -21.33357328978999945, 7.007277454522999882, -6.553624248108999240 ) ) ;
#20418 = ADVANCED_FACE ( 'NONE', ( #10500 ), #3354, .T. ) ;
#20419 = CARTESIAN_POINT ( 'NONE',  ( 11.45478115325934709, -9.254429737870434991, -8.970723317480709724 ) ) ;
#20420 = CARTESIAN_POINT ( 'NONE',  ( -4.823558943698996515, 13.17409018072999238, -5.974474971606000828 ) ) ;
#20421 = CARTESIAN_POINT ( 'NONE',  ( -10.35615758860000035, 7.000000000000000000, 0.000000000000000000 ) ) ;
#20422 = LINE ( 'NONE', #5989, #19343 ) ;
#20423 = CARTESIAN_POINT ( 'NONE',  ( 5.699442596042000098, 1.578914512950999657E-14, 0.000000000000000000 ) ) ;
#20424 = CARTESIAN_POINT ( 'NONE',  ( -5.339911154187996445, 16.17862129490001877, 3.014836506089000334 ) ) ;
#20425 = CARTESIAN_POINT ( 'NONE',  ( -0.6074916215089999350, 30.83999999999999986, -2.072813047478000215 ) ) ;
#20426 = ORIENTED_EDGE ( 'NONE', *, *, #23581, .F. ) ;
#20427 = DIRECTION ( 'NONE',  ( 1.000000000000000000, 0.000000000000000000, 0.000000000000000000 ) ) ;
#20428 = CARTESIAN_POINT ( 'NONE',  ( 14.12234300365937045, 9.014876618753284276, 1.130911957320933858 ) ) ;
#20429 = AXIS2_PLACEMENT_3D ( 'NONE', #9084, #19994, #23624 ) ;
#20430 = CARTESIAN_POINT ( 'NONE',  ( -23.32191191764427529, -0.7265626699458933579, 10.55370311345722634 ) ) ;
#20431 = CARTESIAN_POINT ( 'NONE',  ( -0.2400955718764000157, 26.82687716036000225, -2.437731244915000151 ) ) ;
#20432 = CARTESIAN_POINT ( 'NONE',  ( 1.043766574049543872, 11.52930182343673593, 4.698691617476282723 ) ) ;
#20433 = VERTEX_POINT ( 'NONE', #16399 ) ;
#20434 = CARTESIAN_POINT ( 'NONE',  ( -4.849982476240733753, 12.44999999999999929, -0.4215379369927308995 ) ) ;
#20435 = DIRECTION ( 'NONE',  ( 0.000000000000000000, -1.000000000000000000, -9.414809210018000201E-11 ) ) ;
#20436 = CARTESIAN_POINT ( 'NONE',  ( 2.053005267516999902E-14, 28.63049582772000079, 2.160000000000000142 ) ) ;
#20437 = ORIENTED_EDGE ( 'NONE', *, *, #14930, .T. ) ;
#20438 = DIRECTION ( 'NONE',  ( 0.000000000000000000, 1.000000000000000000, 0.000000000000000000 ) ) ;
#20439 = CIRCLE ( 'NONE', #8865, 1.000000000000000666 ) ;
#20440 = CARTESIAN_POINT ( 'NONE',  ( 16.81987658530999852, -0.9597138970337001362, 10.18860816546999892 ) ) ;
#20441 = CARTESIAN_POINT ( 'NONE',  ( 18.32386509258522267, 7.507573501765766544, -7.224273886700561143 ) ) ;
#20442 = EDGE_CURVE ( 'NONE', #9910, #10482, #8919, .T. ) ;
#20443 = CARTESIAN_POINT ( 'NONE',  ( 1.259047450927257339, 29.30086340285666680, 2.184465970885639763 ) ) ;
#20444 = CARTESIAN_POINT ( 'NONE',  ( -1.303057794327999952, 30.02656693603999827, -1.711078215202000097 ) ) ;
#20445 = DIRECTION ( 'NONE',  ( -1.000000000000000000, 0.000000000000000000, 0.000000000000000000 ) ) ;
#20446 = CARTESIAN_POINT ( 'NONE',  ( -1.398492736905084355, 30.86841771689475777, -1.613912722856696735 ) ) ;
#20447 = ORIENTED_EDGE ( 'NONE', *, *, #12744, .F. ) ;
#20448 = PLANE ( 'NONE',  #12956 ) ;
#20449 = CARTESIAN_POINT ( 'NONE',  ( 20.75000399882000224, 8.798721959408998927, 6.165518250330999983 ) ) ;
#20450 = CIRCLE ( 'NONE', #8076, 2.649999999999999911 ) ;
#20451 = CARTESIAN_POINT ( 'NONE',  ( -24.43053737900748246, 6.547205609487094513, -7.918560603455738089 ) ) ;
#20452 = ORIENTED_EDGE ( 'NONE', *, *, #22278, .T. ) ;
#20453 = CARTESIAN_POINT ( 'NONE',  ( 6.243179582884000212, 1.148189900220999940E-14, 0.000000000000000000 ) ) ;
#20454 = CONICAL_SURFACE ( 'NONE', #10014, 4.674999979945999584, 0.7853981633972997312 ) ;
#20455 = DIRECTION ( 'NONE',  ( -1.000000000000000000, 0.000000000000000000, 0.000000000000000000 ) ) ;
#20456 =( GEOMETRIC_REPRESENTATION_CONTEXT ( 3 ) GLOBAL_UNCERTAINTY_ASSIGNED_CONTEXT ( ( #14513 ) ) GLOBAL_UNIT_ASSIGNED_CONTEXT ( ( #4478, #9804, #11866 ) ) REPRESENTATION_CONTEXT ( 'NONE', 'WORKASPACE' ) );
#20457 = CARTESIAN_POINT ( 'NONE',  ( 2.334980371411002231, 11.67499751873000591, 4.254577570424000754 ) ) ;
#20458 = CARTESIAN_POINT ( 'NONE',  ( -1.235933521449031236, 29.28142108852966885, -1.771341811557728629 ) ) ;
#20459 = EDGE_CURVE ( 'NONE', #5746, #9506, #10148, .T. ) ;
#20460 = CARTESIAN_POINT ( 'NONE',  ( -19.80448867117999967, 7.367983127705000079, 8.228944869744001522 ) ) ;
#20461 = VERTEX_POINT ( 'NONE', #5054 ) ;
#20462 = CLOSED_SHELL ( 'NONE', ( #22269, #11860, #3511, #22140, #6902, #15270, #7634, #20047, #16023, #21101, #21232, #14955, #17351, #19091, #3063, #17110, #18716, #11293, #10272, #15890, #21553, #12352, #11120 ) ) ;
#20463 = FACE_OUTER_BOUND ( 'NONE', #6249, .T. ) ;
#20464 = AXIS2_PLACEMENT_3D ( 'NONE', #13931, #16095, #14413 ) ;
#20465 = ORIENTED_EDGE ( 'NONE', *, *, #11482, .T. ) ;
#20466 = CARTESIAN_POINT ( 'NONE',  ( -2.028744019202999738, 25.29888056986999700, -0.7451492096742999838 ) ) ;
#20467 = CARTESIAN_POINT ( 'NONE',  ( 5.615220178540004881, 13.77392129510000451, 3.559094044476999397 ) ) ;
#20468 = CARTESIAN_POINT ( 'NONE',  ( 0.9334375154566999511, 28.75049822780999875, 1.831974274068000064 ) ) ;
#20469 = CARTESIAN_POINT ( 'NONE',  ( 16.50495603379667031, -4.580212439236231781, 7.946988475063720969 ) ) ;
#20470 = DIRECTION ( 'NONE',  ( -1.000000000000000000, 0.000000000000000000, 0.000000000000000000 ) ) ;
#20471 = FACE_BOUND ( 'NONE', #16557, .T. ) ;
#20472 = CARTESIAN_POINT ( 'NONE',  ( 15.85912674931000055, -8.678267488395999152, -6.289192543930000490 ) ) ;
#20473 = CIRCLE ( 'NONE', #18154, 4.750000000000000000 ) ;
#20474 = CARTESIAN_POINT ( 'NONE',  ( -16.77363468649999945, -9.766024879818999693, 0.2197783339474000119 ) ) ;
#20475 = FACE_OUTER_BOUND ( 'NONE', #8971, .T. ) ;
#20476 = VECTOR ( 'NONE', #4217, 1000.000000000000227 ) ;
#20477 = DIRECTION ( 'NONE',  ( 0.000000000000000000, 0.000000000000000000, -1.000000000000000000 ) ) ;
#20478 = EDGE_CURVE ( 'NONE', #9831, #4023, #1493, .T. ) ;
#20479 = ORIENTED_EDGE ( 'NONE', *, *, #22112, .F. ) ;
#20480 = CARTESIAN_POINT ( 'NONE',  ( -21.53391127295000018, -1.797407140843000128, 11.09281522174999957 ) ) ;
#20481 = CARTESIAN_POINT ( 'NONE',  ( 1.619437063074000038, 24.08748676817999979, -1.682281432622000139 ) ) ;
#20482 = CARTESIAN_POINT ( 'NONE',  ( 14.09191795553696913, -9.926564809749867990, -2.934343053110770594 ) ) ;
#20483 = VECTOR ( 'NONE', #6209, 1000.000000000000000 ) ;
#20484 = DIRECTION ( 'NONE',  ( 0.000000000000000000, -0.8660254037844288266, 0.5000000000000169864 ) ) ;
#20485 = CARTESIAN_POINT ( 'NONE',  ( 23.86849505023999996, 10.71391760736999998, -3.584493356444999890 ) ) ;
#20486 = CARTESIAN_POINT ( 'NONE',  ( -2.355876953200999768, 29.97705122577999859, -0.1484490314924999943 ) ) ;
#20487 = CARTESIAN_POINT ( 'NONE',  ( 13.79821159651314311, 9.024933071421822106, -0.1076915288274838262 ) ) ;
#20488 = CARTESIAN_POINT ( 'NONE',  ( 0.000000000000000000, 26.50000000000000000, 0.000000000000000000 ) ) ;
#20489 = DIRECTION ( 'NONE',  ( 0.000000000000000000, 1.000000000000000000, 0.000000000000000000 ) ) ;
#20490 = CIRCLE ( 'NONE', #20101, 7.000000000000000000 ) ;
#20491 = ADVANCED_FACE ( 'NONE', ( #3931 ), #10697, .F. ) ;
#20492 = CARTESIAN_POINT ( 'NONE',  ( 22.84441020264000244, -10.91804186159999901, 3.505057996334000503 ) ) ;
#20493 = VERTEX_POINT ( 'NONE', #15055 ) ;
#20494 = CARTESIAN_POINT ( 'NONE',  ( -0.7554624816769099915, 24.39581436972834538, 2.418296485626394876 ) ) ;
#20495 = CARTESIAN_POINT ( 'NONE',  ( 0.1784790855350541217, 29.74995697614779644, -4.515757205439222766 ) ) ;
#20496 = AXIS2_PLACEMENT_3D ( 'NONE', #4755, #6435, #13945 ) ;
#20497 = ORIENTED_EDGE ( 'NONE', *, *, #4648, .T. ) ;
#20498 = DIRECTION ( 'NONE',  ( -1.000000000000000000, 0.000000000000000000, 0.000000000000000000 ) ) ;
#20499 = DIRECTION ( 'NONE',  ( -1.000000000000000000, 0.000000000000000000, 0.000000000000000000 ) ) ;
#20500 = CARTESIAN_POINT ( 'NONE',  ( -2.649379677059598759, 28.02555747447239654, -3.089210087443399200 ) ) ;
#20501 = CARTESIAN_POINT ( 'NONE',  ( 19.13672573371000141, -5.603022739495999716, 8.809601378027998919 ) ) ;
#20502 = CARTESIAN_POINT ( 'NONE',  ( -17.43032910583999850, 9.118578311265999048, 0.000000000000000000 ) ) ;
#20503 = CARTESIAN_POINT ( 'NONE',  ( 2.254114612530000006, 25.55756359724000149, 0.5071914623444000458 ) ) ;
#20504 = ORIENTED_EDGE ( 'NONE', *, *, #6996, .F. ) ;
#20505 = ORIENTED_EDGE ( 'NONE', *, *, #21491, .T. ) ;
#20506 = CARTESIAN_POINT ( 'NONE',  ( -11.52355113877000115, -6.819129568044999701, 13.60514851516999890 ) ) ;
#20507 = FACE_OUTER_BOUND ( 'NONE', #20911, .T. ) ;
#20508 = CARTESIAN_POINT ( 'NONE',  ( -14.47158024777374052, -9.790304928767106674, -8.042633409158213453 ) ) ;
#20509 = EDGE_CURVE ( 'NONE', #7192, #1429, #8760, .T. ) ;
#20510 = VERTEX_POINT ( 'NONE', #16641 ) ;
#20511 = ADVANCED_FACE ( 'NONE', ( #9615 ), #18779, .T. ) ;
#20512 = CARTESIAN_POINT ( 'NONE',  ( -24.41513307467224436, 9.801374016728995997, 8.023466425259611512 ) ) ;
#20513 = CARTESIAN_POINT ( 'NONE',  ( 4.834780805419000238, 12.45065217972999960, 0.000000000000000000 ) ) ;
#20514 = FACE_BOUND ( 'NONE', #3289, .T. ) ;
#20515 = CARTESIAN_POINT ( 'NONE',  ( 16.03895867897560734, -7.582969449584280319, -7.062017480966269467 ) ) ;
#20516 = CARTESIAN_POINT ( 'NONE',  ( -17.65609590006000218, -11.00188783733999998, 1.405720899317999928 ) ) ;
#20517 = CARTESIAN_POINT ( 'NONE',  ( -1.096889435125999901, 30.16030992228000329, 2.085328208951000128 ) ) ;
#20518 = CARTESIAN_POINT ( 'NONE',  ( -15.02697771723000031, -1.474210749020000044, -10.68967233462999999 ) ) ;
#20519 = CARTESIAN_POINT ( 'NONE',  ( 0.2333643206754606458, 29.61748404124761791, 2.147376024278286444 ) ) ;
#20520 = EDGE_CURVE ( 'NONE', #17141, #6384, #223, .T. ) ;
#20521 = VERTEX_POINT ( 'NONE', #22326 ) ;
#20522 = CARTESIAN_POINT ( 'NONE',  ( 2.043066369328000231, 24.94995867995000083, 1.131945607266999998 ) ) ;
#20523 = EDGE_CURVE ( 'NONE', #15500, #1220, #19973, .T. ) ;
#20524 = CARTESIAN_POINT ( 'NONE',  ( 20.21412898074317965, 9.226432912327343416, -5.052731391976187147 ) ) ;
#20525 = DIRECTION ( 'NONE',  ( -0.000000000000000000, -1.000000000000000000, -0.000000000000000000 ) ) ;
#20526 = EDGE_LOOP ( 'NONE', ( #18629, #3539, #2472, #3759 ) ) ;
#20527 = PLANE ( 'NONE',  #14300 ) ;
#20528 = CARTESIAN_POINT ( 'NONE',  ( -23.75701756406583343, -13.93375672974000068, 0.3849425536981887497 ) ) ;
#20529 = CARTESIAN_POINT ( 'NONE',  ( 17.56125142131000061, 3.538711643716999866, -9.078802261343000168 ) ) ;
#20530 = ORIENTED_EDGE ( 'NONE', *, *, #2779, .T. ) ;
#20531 = CARTESIAN_POINT ( 'NONE',  ( -14.25851234816000002, 6.967815116019000499, -12.06644646457999848 ) ) ;
#20532 = CARTESIAN_POINT ( 'NONE',  ( -14.44097977832075941, 2.973612400766980635, -12.49999313495041697 ) ) ;
#20533 = ORIENTED_EDGE ( 'NONE', *, *, #9515, .T. ) ;
#20534 = CARTESIAN_POINT ( 'NONE',  ( -23.23831814003093399, 2.819964850040427518, -8.988637406128791696 ) ) ;
#20535 = CARTESIAN_POINT ( 'NONE',  ( -4.694474657144001029, 12.59750342685999591, 1.086550191527999143 ) ) ;
#20536 = VECTOR ( 'NONE', #11504, 1000.000000000000000 ) ;
#20537 = CARTESIAN_POINT ( 'NONE',  ( 12.00000000000000000, -2.090383947266901465, -9.242149839633347241 ) ) ;
#20538 = CARTESIAN_POINT ( 'NONE',  ( 19.49049770046332242, 9.171446297783335311, -1.200666460651649947 ) ) ;
#20539 = CARTESIAN_POINT ( 'NONE',  ( 0.000000000000000000, 23.00000000000000000, 0.000000000000000000 ) ) ;
#20540 = PLANE ( 'NONE',  #4265 ) ;
#20541 = SURFACE_STYLE_FILL_AREA ( #13501 ) ;
#20542 = CARTESIAN_POINT ( 'NONE',  ( 1.259047450927247569, 27.96753006952333465, -2.184465970885645536 ) ) ;
#20543 = CARTESIAN_POINT ( 'NONE',  ( 0.8998430216380005620, 30.45864892563614745, 1.963489132376946333 ) ) ;
#20544 = ORIENTED_EDGE ( 'NONE', *, *, #14987, .F. ) ;
#20545 = CARTESIAN_POINT ( 'NONE',  ( 23.07322687843999987, 9.811823008121001166, -1.038166454746999978 ) ) ;
#20546 = B_SPLINE_CURVE_WITH_KNOTS ( 'NONE', 3,
 ( #5249, #12633, #1001, #8402, #18432, #22180, #7518, #11169, #9229, #4011, #18, #1960, #14902, #20494, #11290, #22293, #9465, #7647 ),
 .UNSPECIFIED., .F., .F.,
 ( 4, 2, 2, 2, 2, 2, 2, 2, 4 ),
 ( 0.000000000000000000, 0.09854977542085557873, 0.1970995508417111575, 0.2956493262625667362, 0.3941991016834223149, 0.4927488771042778937, 0.5912986525251334724, 0.6898484279459891066, 0.7883982033668446299 ),
 .UNSPECIFIED. ) ;
#20547 = CARTESIAN_POINT ( 'NONE',  ( 14.49567727038531650, 1.385394744686596846, 8.990065437785395019 ) ) ;
#20548 = CARTESIAN_POINT ( 'NONE',  ( 0.000000000000000000, 16.94999982584599962, 0.000000000000000000 ) ) ;
#20549 = CARTESIAN_POINT ( 'NONE',  ( -0.5788358281067000899, 25.82114211381999880, -2.218121370661999769 ) ) ;
#20550 = CARTESIAN_POINT ( 'NONE',  ( -0.3463667137703017040, 28.20780860099542053, 4.418706525546099328 ) ) ;
#20551 = VERTEX_POINT ( 'NONE', #22448 ) ;
#20552 = CARTESIAN_POINT ( 'NONE',  ( -2.792997288517848897, 11.81229427091517792, -3.933476770808612244 ) ) ;
#20553 = LINE ( 'NONE', #9299, #14959 ) ;
#20554 = DIRECTION ( 'NONE',  ( 0.9771428571428639742, 0.000000000000000000, -0.2125837170026919909 ) ) ;
#20555 = ORIENTED_EDGE ( 'NONE', *, *, #16173, .T. ) ;
#20556 = CARTESIAN_POINT ( 'NONE',  ( 13.52925158531000172, -9.668754250937999117, 3.079128054934999525 ) ) ;
#20557 = CARTESIAN_POINT ( 'NONE',  ( 24.50000000000000000, 4.174438572590999431E-14, -12.50000000000000000 ) ) ;
#20558 = FACE_OUTER_BOUND ( 'NONE', #1293, .T. ) ;
#20559 = CARTESIAN_POINT ( 'NONE',  ( 15.53114037305999950, 2.007458543610999957, 10.62532755895000136 ) ) ;
#20560 = CARTESIAN_POINT ( 'NONE',  ( 13.50000000000000178, -7.707699124303561078, -5.256970985969869226 ) ) ;
#20561 = CARTESIAN_POINT ( 'NONE',  ( 0.000000000000000000, 26.50000000000000355, 4.000000000000614619 ) ) ;
#20562 = CARTESIAN_POINT ( 'NONE',  ( 22.87459322467000078, -1.252498931826999895, 10.72907436738999998 ) ) ;
#20563 = VECTOR ( 'NONE', #3367, 1000.000000000000227 ) ;
#20564 = FACE_OUTER_BOUND ( 'NONE', #4928, .T. ) ;
#20565 = ORIENTED_EDGE ( 'NONE', *, *, #8212, .T. ) ;
#20566 = DIRECTION ( 'NONE',  ( 0.000000000000000000, -1.000000000000000000, 0.000000000000000000 ) ) ;
#20567 = DIRECTION ( 'NONE',  ( 0.000000000000000000, -1.000000000000000000, 0.000000000000000000 ) ) ;
#20568 = CARTESIAN_POINT ( 'NONE',  ( 4.833443960760002156, 12.42174102045999895, -0.1521463468820001830 ) ) ;
#20569 = CARTESIAN_POINT ( 'NONE',  ( -1.246714904460894946, 29.28220451215178599, -1.763772490062673892 ) ) ;
#20570 = CARTESIAN_POINT ( 'NONE',  ( -24.12822391257000021, 5.443199013828000865, -9.745701579671997905 ) ) ;
#20571 = VERTEX_POINT ( 'NONE', #5860 ) ;
#20572 = CARTESIAN_POINT ( 'NONE',  ( 0.000000000000000000, 15.00000000000000000, -4.625000000000000000 ) ) ;
#20573 = AXIS2_PLACEMENT_3D ( 'NONE', #16112, #18418, #1827 ) ;
#20574 = VERTEX_POINT ( 'NONE', #17000 ) ;
#20575 = EDGE_CURVE ( 'NONE', #11791, #21237, #1407, .T. ) ;
#20576 = CARTESIAN_POINT ( 'NONE',  ( 1.903337834367000214, 24.88085889271999562, 1.023891906906999827 ) ) ;
#20577 = DIRECTION ( 'NONE',  ( 0.000000000000000000, 1.000000000000000000, 0.000000000000000000 ) ) ;
#20578 = CARTESIAN_POINT ( 'NONE',  ( -4.000000000000000000, 28.30000000000000071, -2.309401076759000304 ) ) ;
#20579 = DIRECTION ( 'NONE',  ( 1.000000000000000000, 0.000000000000000000, 0.000000000000000000 ) ) ;
#20580 = CARTESIAN_POINT ( 'NONE',  ( 18.93264468355999952, 0.000000000000000000, 0.000000000000000000 ) ) ;
#20581 = DIRECTION ( 'NONE',  ( -1.000000000000000000, 0.000000000000000000, 0.000000000000000000 ) ) ;
#20582 = CARTESIAN_POINT ( 'NONE',  ( 15.20100174931000048, 0.8726850093137999975, 10.66462197497000020 ) ) ;
#20583 =( NAMED_UNIT ( * ) SI_UNIT ( $, .STERADIAN. ) SOLID_ANGLE_UNIT ( ) );
#20584 = CARTESIAN_POINT ( 'NONE',  ( -15.39248033193999987, -8.001506135565000122, 6.430926145009000727 ) ) ;
#20585 = CIRCLE ( 'NONE', #22512, 2.729128784747790970 ) ;
#20586 = CYLINDRICAL_SURFACE ( 'NONE', #9384, 5.000000000000004441 ) ;
#20587 = CARTESIAN_POINT ( 'NONE',  ( -14.42499035157292298, 3.357933904594045948, 12.49997221285009452 ) ) ;
#20588 = ORIENTED_EDGE ( 'NONE', *, *, #8923, .F. ) ;
#20589 = EDGE_CURVE ( 'NONE', #18102, #23527, #18557, .T. ) ;
#20590 = CARTESIAN_POINT ( 'NONE',  ( 2.532323260332000281, 30.01197222537999920, 1.003311987937999916 ) ) ;
#20591 = CARTESIAN_POINT ( 'NONE',  ( -1.199980338850999972, 24.94266885362000252, -2.222287597575000273 ) ) ;
#20592 = CARTESIAN_POINT ( 'NONE',  ( 13.69973086387940242, -4.969862238816942224, 9.044112284830802651 ) ) ;
#20593 = CARTESIAN_POINT ( 'NONE',  ( -11.00000000000000000, -10.59999999999999964, 0.000000000000000000 ) ) ;
#20594 = CARTESIAN_POINT ( 'NONE',  ( 24.19866361008999789, 10.75771654126000065, 3.480411140149000104 ) ) ;
#20595 = CARTESIAN_POINT ( 'NONE',  ( 1.523522810973999997, 29.47438902658999993, 1.803072815451999933 ) ) ;
#20596 = CARTESIAN_POINT ( 'NONE',  ( 14.37697681739622091, -3.685858481565998268, 8.257677185639298756 ) ) ;
#20597 = CARTESIAN_POINT ( 'NONE',  ( 20.43528936713000377, -9.195691514035999603, 0.000000000000000000 ) ) ;
#20598 = CARTESIAN_POINT ( 'NONE',  ( -6.559180854920310111, 15.42694216100158044, 1.532439657023070723 ) ) ;
#20599 = CARTESIAN_POINT ( 'NONE',  ( 11.07373617190084403, 10.57520287783416002, -6.683140124535795756 ) ) ;
#20600 = VERTEX_POINT ( 'NONE', #8406 ) ;
#20601 = VECTOR ( 'NONE', #9829, 1000.000000000000000 ) ;
#20602 = DIRECTION ( 'NONE',  ( -1.000000000000000000, 0.000000000000000000, 0.000000000000000000 ) ) ;
#20603 = B_SPLINE_CURVE_WITH_KNOTS ( 'NONE', 3,
 ( #16099, #14181, #10910, #14416, #4990, #21923, #21579, #10674, #16232, #21809, #10796, #1591 ),
 .UNSPECIFIED., .F., .F.,
 ( 4, 2, 2, 2, 2, 4 ),
 ( 0.000000000000000000, 0.2499999999999396039, 0.3749999999999250599, 0.4374999999999310552, 0.4999999999999370504, 1.000000000000000000 ),
 .UNSPECIFIED. ) ;
#20604 = ORIENTED_EDGE ( 'NONE', *, *, #12962, .F. ) ;
#20605 = EDGE_CURVE ( 'NONE', #8738, #11139, #11446, .T. ) ;
#20606 = B_SPLINE_SURFACE_WITH_KNOTS ( 'NONE', 3, 3, ( 
 ( #1267, #14098, #21493, #3097, #16018, #23412, #10600, #1387, #16142, #22548, #8267, #19407, #6071, #20979, #17103, #9721, #8020, #745, #22782, #15631, #16985, #21225, #387, #11780, #7784, #15514, #15153, #5955, #19154, #11543, #8149, #9956, #22902, #13462, #2564 ),
 ( #501, #4147, #20865, #6318, #4275, #21096, #18923, #11901, #2332, #7902, #15271, #11663, #19035, #2445, #9837, #17219, #617, #15876, #1361, #21467, #8750, #5238, #10571, #21344, #23144, #1484, #19533, #2939, #10688, #5009, #8389, #14072, #16115, #1115, #4880 ),
 ( #6566, #23517, #21594, #18077, #17957, #6928, #17843, #19891, #12395, #13950, #988, #3307, #15755, #10455, #6680, #7047, #8517, #3189, #12623, #8628, #8878, #19779, #14324, #21713, #4759, #12145, #5123, #14430, #15991, #12506, #16248, #23640, #21825, #12268, #23266 ),
 ( #20007, #19655, #10327, #17594, #10201, #17718, #3070, #1237, #23384, #6803, #14196, #5695, #13080, #16596, #11037, #12961, #5349, #13197, #2062, #12849, #20480, #3888, #18420, #11155, #14544, #22058, #5467, #11279, #18656, #15008, #20245, #18541, #12738, #14663, #7631 ) ),
 .UNSPECIFIED., .F., .F., .F.,
 ( 4, 4 ),
 ( 4, 1, 1, 1, 1, 1, 1, 1, 1, 1, 1, 1, 1, 1, 1, 1, 1, 1, 1, 1, 1, 1, 1, 1, 1, 1, 1, 1, 1, 1, 1, 1, 4 ),
 ( -0.08408083179840999954, 1.084080831798000188 ),
 ( 0.1394980018163999858, 0.1669159576409000034, 0.1943339134653999933, 0.2217518692897999799, 0.2491698251142999976, 0.2765877809387999875, 0.3040057367633000052, 0.3314236925876999917, 0.3588416484122000094, 0.3862596042366999716, 0.4136775600611999892, 0.4410955158857000069, 0.4685134717100999935, 0.4959314275345999556, 0.5233493833590999733, 0.5507673391835999910, 0.5781852950080000886, 0.6056032508324999952, 0.6330212066570000129, 0.6604391624814999195, 0.6878571183060000482, 0.7152750741304000348, 0.7426930299549000525, 0.7701109857793999591, 0.7975289416039000878, 0.8249468974282999634, 0.8523648532527999810, 0.8797828090773001097, 0.9072007649018000164, 0.9346187207262000030, 0.9620366765507000206, 0.9894546323751999273, 1.016872588200000038 ),
 .UNSPECIFIED. ) ;
#20607 = CARTESIAN_POINT ( 'NONE',  ( 0.000000000000000000, 18.50000000000000000, 0.000000000000000000 ) ) ;
#20608 = DIRECTION ( 'NONE',  ( 0.000000000000000000, 1.000000000000000000, 0.000000000000000000 ) ) ;
#20609 = CARTESIAN_POINT ( 'NONE',  ( -23.74465998031000069, -6.216878364870000340, -12.50000000000000000 ) ) ;
#20610 = CARTESIAN_POINT ( 'NONE',  ( 13.27582570505999904, 3.894665007329999540, 9.762755509399999809 ) ) ;
#20611 = CARTESIAN_POINT ( 'NONE',  ( -14.25243324638999809, -7.716878364870000340, -11.63397459621999985 ) ) ;
#20612 = CARTESIAN_POINT ( 'NONE',  ( -1.394936847711000016, 28.14962896667000081, -2.276308483783000103 ) ) ;
#20613 = ORIENTED_EDGE ( 'NONE', *, *, #2998, .F. ) ;
#20614 = ORIENTED_EDGE ( 'NONE', *, *, #12449, .F. ) ;
#20615 = LINE ( 'NONE', #19031, #10340 ) ;
#20616 = CARTESIAN_POINT ( 'NONE',  ( -2.184465970885646424, 27.36753006952333322, -1.259047450927245126 ) ) ;
#20617 = CARTESIAN_POINT ( 'NONE',  ( -0.7783053373570000266, 28.00000000000000000, 6.000000000000000000 ) ) ;
#20618 = CARTESIAN_POINT ( 'NONE',  ( 18.22028936713000036, -1.652712406954000013, 8.988165862088999702 ) ) ;
#20619 = ORIENTED_EDGE ( 'NONE', *, *, #14448, .F. ) ;
#20620 = EDGE_CURVE ( 'NONE', #14405, #1761, #9854, .T. ) ;
#20621 = CARTESIAN_POINT ( 'NONE',  ( -14.45561352951336609, 12.11761689492931282, 4.011600805608035891 ) ) ;
#20622 = CARTESIAN_POINT ( 'NONE',  ( 20.38206396265981368, 7.578948228821809963, 7.305733806372995076 ) ) ;
#20623 = CARTESIAN_POINT ( 'NONE',  ( 6.195288800946270769, 13.89803996554030974, 0.8525294906254528016 ) ) ;
#20624 = CARTESIAN_POINT ( 'NONE',  ( 15.75587683109987580, -10.06225463003949194, 2.437168688431326391 ) ) ;
#20625 = CARTESIAN_POINT ( 'NONE',  ( -16.78682104303999978, 7.979255941467000568, -7.669513122050999776 ) ) ;
#20626 = CARTESIAN_POINT ( 'NONE',  ( 1.466483324883999906, 29.69536550879999837, -1.630154757756000050 ) ) ;
#20627 = CARTESIAN_POINT ( 'NONE',  ( -18.31782136596999777, 10.89202446812999980, 3.425794516969999925 ) ) ;
#20628 = EDGE_CURVE ( 'NONE', #7085, #19479, #15645, .T. ) ;
#20629 = CARTESIAN_POINT ( 'NONE',  ( 0.9925186210581510293, 29.66472845694044125, 1.918284758963818559 ) ) ;
#20630 = ORIENTED_EDGE ( 'NONE', *, *, #13519, .T. ) ;
#20631 = CARTESIAN_POINT ( 'NONE',  ( -1.674130751070000089, 23.92133400015999811, 1.398636182056999910 ) ) ;
#20632 = LINE ( 'NONE', #21080, #14677 ) ;
#20633 = DIRECTION ( 'NONE',  ( 0.000000000000000000, -1.000000000000000000, 0.000000000000000000 ) ) ;
#20634 = ORIENTED_EDGE ( 'NONE', *, *, #16453, .F. ) ;
#20635 = EDGE_CURVE ( 'NONE', #23530, #17452, #3357, .T. ) ;
#20636 = CARTESIAN_POINT ( 'NONE',  ( 24.50000000000001066, -1.022558425349066269, 12.50000000000000533 ) ) ;
#20637 = CARTESIAN_POINT ( 'NONE',  ( -0.4221993467342085582, 30.45569945603167739, -2.502179599253123055 ) ) ;
#20638 = EDGE_CURVE ( 'NONE', #19945, #2909, #17399, .T. ) ;
#20639 = CARTESIAN_POINT ( 'NONE',  ( -13.99999999999999822, -9.939587166035000365, 2.689278564876886435 ) ) ;
#20640 = CARTESIAN_POINT ( 'NONE',  ( 12.59887625730999972, 2.316137192978999781, 8.804988873405999783 ) ) ;
#20641 = ORIENTED_EDGE ( 'NONE', *, *, #4070, .T. ) ;
#20642 = CARTESIAN_POINT ( 'NONE',  ( -6.310601434888994277, 16.13748856436002654, -0.9718497405647000820 ) ) ;
#20643 = LINE ( 'NONE', #644, #3256 ) ;
#20644 = VECTOR ( 'NONE', #12557, 1000.000000000000227 ) ;
#20645 = ORIENTED_EDGE ( 'NONE', *, *, #9282, .T. ) ;
#20646 = EDGE_CURVE ( 'NONE', #16380, #22057, #878, .T. ) ;
#20647 = CARTESIAN_POINT ( 'NONE',  ( -15.98834587121332795, 8.845253692700577375, -2.376965543786443202 ) ) ;
#20648 = DIRECTION ( 'NONE',  ( 0.7071067811823850136, 0.7071067811898851252, 1.080116765722976056E-06 ) ) ;
#20649 = CARTESIAN_POINT ( 'NONE',  ( 0.8060258553945994775, 11.68578183133999282, 4.773271256242001215 ) ) ;
#20650 = CARTESIAN_POINT ( 'NONE',  ( 12.00000000000000000, -1.414133744360243083, -9.331047239918021319 ) ) ;
#20651 = CARTESIAN_POINT ( 'NONE',  ( 23.41677564524290744, 37.01856778792605240, -6.000000000000000000 ) ) ;
#20652 = CARTESIAN_POINT ( 'NONE',  ( -4.588766208978104721, 13.47548078768067192, 5.171706116033917056 ) ) ;
#20653 = CARTESIAN_POINT ( 'NONE',  ( 0.6100901480019267353, 26.47309547025852439, -2.313337588001243006 ) ) ;
#20654 = CARTESIAN_POINT ( 'NONE',  ( -2.434931691670790155, 29.00086340285666608, -0.6543697108981963995 ) ) ;
#20656 = AXIS2_PLACEMENT_3D ( 'NONE', #6354, #9871, #10237 ) ;
#20655 = CYLINDRICAL_SURFACE ( 'NONE', #1806, 1.750000000000000000 ) ;
#20657 = CARTESIAN_POINT ( 'NONE',  ( 1.295298327500748581, 30.48557000331402733, 1.732529484320999069 ) ) ;
#20658 = ORIENTED_EDGE ( 'NONE', *, *, #19013, .T. ) ;
#20659 = CARTESIAN_POINT ( 'NONE',  ( -17.50591243917333983, 8.883183840251577479, -2.387158987722542314 ) ) ;
#20660 = CARTESIAN_POINT ( 'NONE',  ( 23.12578860888000065, 7.434166750538000912, -7.277889744973999875 ) ) ;
#20661 = CARTESIAN_POINT ( 'NONE',  ( 0.8894771940131762644, 12.83047529882638926, -6.611550444528325521 ) ) ;
#20662 = LINE ( 'NONE', #22351, #23897 ) ;
#20663 = ADVANCED_FACE ( 'NONE', ( #13717 ), #13359, .T. ) ;
#20664 = CARTESIAN_POINT ( 'NONE',  ( -23.08092454245977976, -8.305383183722334195, 6.545568425691888237 ) ) ;
#20665 = CARTESIAN_POINT ( 'NONE',  ( 1.808910716397999829, 27.31696440326000186, -1.672139866504000150 ) ) ;
#20666 = VECTOR ( 'NONE', #11565, 1000.000000000000000 ) ;
#20667 = DIRECTION ( 'NONE',  ( 0.000000000000000000, -1.000000000000000000, 0.000000000000000000 ) ) ;
#20668 = ORIENTED_EDGE ( 'NONE', *, *, #20798, .T. ) ;
#20669 = CARTESIAN_POINT ( 'NONE',  ( -17.29360359819550297, -9.005800717077383055, -5.261463894023568955 ) ) ;
#20670 = CARTESIAN_POINT ( 'NONE',  ( 23.99478584078000054, -7.550251870568999379, -11.73017644755000077 ) ) ;
#20671 = AXIS2_PLACEMENT_3D ( 'NONE', #10112, #2599, #9991 ) ;
#20672 = DIRECTION ( 'NONE',  ( -1.000000000000000000, 0.000000000000000000, 0.000000000000000000 ) ) ;
#20673 = ORIENTED_EDGE ( 'NONE', *, *, #15278, .T. ) ;
#20674 = EDGE_CURVE ( 'NONE', #8671, #4654, #11910, .T. ) ;
#20675 = DIRECTION ( 'NONE',  ( -1.000000000000000000, 0.000000000000000000, 0.000000000000000000 ) ) ;
#20676 = B_SPLINE_CURVE_WITH_KNOTS ( 'NONE', 3,
 ( #6314, #19530, #17715, #13701, #21093, #4505, #11897, #12024 ),
 .UNSPECIFIED., .F., .F.,
 ( 4, 2, 2, 4 ),
 ( 0.000000000000000000, 0.2500000000000000000, 0.5000000000000000000, 1.000000000000000000 ),
 .UNSPECIFIED. ) ;
#20677 = CIRCLE ( 'NONE', #10246, 4.724999999999999645 ) ;
#20678 = CARTESIAN_POINT ( 'NONE',  ( 12.43237658531000100, 5.753414546153999609, -8.323445001914000940 ) ) ;
#20679 = CARTESIAN_POINT ( 'NONE',  ( -17.59444652563999867, -11.39502044605000108, 0.2566590569923999920 ) ) ;
#20680 = LINE ( 'NONE', #22370, #13102 ) ;
#20681 = CARTESIAN_POINT ( 'NONE',  ( 14.24421080085999947, -6.039990374987000088, -9.570627441890000142 ) ) ;
#20682 = CARTESIAN_POINT ( 'NONE',  ( 13.49999999999999822, -8.457508417532315192, -4.109938046728712990 ) ) ;
#20683 = DIRECTION ( 'NONE',  ( 0.000000000000000000, 0.000000000000000000, -1.000000000000000000 ) ) ;
#20684 = CARTESIAN_POINT ( 'NONE',  ( 24.03114330764999806, 0.4208889323872999633, -10.29577946621999907 ) ) ;
#20685 = CARTESIAN_POINT ( 'NONE',  ( 3.000000000000000000, 20.00000000000000000, 0.000000000000000000 ) ) ;
#20686 = ORIENTED_EDGE ( 'NONE', *, *, #15224, .F. ) ;
#20687 = CARTESIAN_POINT ( 'NONE',  ( -14.25243324638999809, -6.216878364870000340, -12.50000000000000000 ) ) ;
#20688 = CARTESIAN_POINT ( 'NONE',  ( 2.669209039122999894, 27.55206776952000070, 0.05241653317053000111 ) ) ;
#20689 = AXIS2_PLACEMENT_3D ( 'NONE', #2943, #23644, #12272 ) ;
#20690 = CARTESIAN_POINT ( 'NONE',  ( -3.189163304378001218, 11.94355460396000268, 3.580087194034999865 ) ) ;
#20691 = CARTESIAN_POINT ( 'NONE',  ( 2.155476837356603781, 28.99572802833808538, 0.1381959937958471552 ) ) ;
#20692 = CARTESIAN_POINT ( 'NONE',  ( -23.10525368899999776, -11.00684294169000133, 1.684798661880999804 ) ) ;
#20693 = ORIENTED_EDGE ( 'NONE', *, *, #5938, .T. ) ;
#20694 = DIRECTION ( 'NONE',  ( 0.000000000000000000, 1.000000000000000000, 0.000000000000000000 ) ) ;
#20695 = VERTEX_POINT ( 'NONE', #517 ) ;
#20696 = CARTESIAN_POINT ( 'NONE',  ( -24.50000000000453326, 0.5124611672102585835, -12.50000000000234301 ) ) ;
#20697 = CARTESIAN_POINT ( 'NONE',  ( 1.254873950010960026, 11.63135044190335599, 4.623136993607071865 ) ) ;
#20698 = CARTESIAN_POINT ( 'NONE',  ( -0.5724186824819998964, 25.92299822780999818, -2.193530619437999984 ) ) ;
#20699 = DIRECTION ( 'NONE',  ( 0.000000000000000000, -1.000000000000000000, 0.000000000000000000 ) ) ;
#20700 = DIRECTION ( 'NONE',  ( 0.000000000000000000, 1.000000000000000000, 0.000000000000000000 ) ) ;
#20701 = CARTESIAN_POINT ( 'NONE',  ( 15.74943924931000083, -10.38900229657999930, -2.621660623529000311 ) ) ;
#20702 = CARTESIAN_POINT ( 'NONE',  ( -18.48019363270999804, 4.914628609928000103, -9.714689191606000307 ) ) ;
#20703 = CIRCLE ( 'NONE', #6792, 0.09999999999999939493 ) ;
#20704 = CARTESIAN_POINT ( 'NONE',  ( 4.000000000000000000, 28.30000000000000071, -2.309401076759000304 ) ) ;
#20705 = CARTESIAN_POINT ( 'NONE',  ( -14.46758738532042798, 2.198682497491741383, 12.49996900094042473 ) ) ;
#20706 = VERTEX_POINT ( 'NONE', #22677 ) ;
#20707 = CARTESIAN_POINT ( 'NONE',  ( -4.000000000000001776, 29.97444252552741872, 0.7494995952805654227 ) ) ;
#20708 = CARTESIAN_POINT ( 'NONE',  ( -2.413984953566000069, 23.46972322239999897, -0.1881867403046000031 ) ) ;
#20709 = CARTESIAN_POINT ( 'NONE',  ( 14.31900924450000723, -4.887163463281674503, -9.111456757049891664 ) ) ;
#20710 = CARTESIAN_POINT ( 'NONE',  ( 2.121949948620001081, 12.82851042524998597, -6.764654941373005492 ) ) ;
#20711 = FACE_OUTER_BOUND ( 'NONE', #21685, .T. ) ;
#20712 = ADVANCED_FACE ( 'NONE', ( #23765 ), #16859, .F. ) ;
#20713 = CARTESIAN_POINT ( 'NONE',  ( 1.661669601868999813, 28.68449128500000000, 1.676656731525000055 ) ) ;
#20714 = CARTESIAN_POINT ( 'NONE',  ( 14.68340655888479596, -9.046510072424961635, 0.7085215494182042217 ) ) ;
#20715 = FACE_OUTER_BOUND ( 'NONE', #14708, .T. ) ;
#20716 = DIRECTION ( 'NONE',  ( -0.7071067811905932254, 0.7071067811824932603, -1.099460837533990473E-07 ) ) ;
#20717 = VECTOR ( 'NONE', #9747, 1000.000000000000000 ) ;
#20718 = CARTESIAN_POINT ( 'NONE',  ( 24.38510397947349162, -12.27045979993889802, -3.746940194273108204 ) ) ;
#20719 = ORIENTED_EDGE ( 'NONE', *, *, #2453, .T. ) ;
#20720 = CARTESIAN_POINT ( 'NONE',  ( -2.000000000000000000, 24.50000000000000000, -3.464101615137999968 ) ) ;
#20721 = TOROIDAL_SURFACE ( 'NONE', #22270, 2.100000000000000089, 0.1000000000000000056 ) ;
#20722 = CARTESIAN_POINT ( 'NONE',  ( 66.60588651278291650, 37.01856778792605240, -1.000000000000000000 ) ) ;
#20723 = VERTEX_POINT ( 'NONE', #1617 ) ;
#20724 = CARTESIAN_POINT ( 'NONE',  ( 2.733205704442000172, 25.26683306396000006, -0.1467716043025000250 ) ) ;
#20725 = CARTESIAN_POINT ( 'NONE',  ( 0.000000000000000000, 30.00000000000000000, 0.000000000000000000 ) ) ;
#20726 = B_SPLINE_CURVE_WITH_KNOTS ( 'NONE', 3,
 ( #10569, #2697, #12025, #862 ),
 .UNSPECIFIED., .F., .F.,
 ( 4, 4 ),
 ( 0.000000000000000000, 1.000000000000000000 ),
 .UNSPECIFIED. ) ;
#20727 = CARTESIAN_POINT ( 'NONE',  ( 0.7453833240861579279, 24.57675687152185873, 2.221003709730194675 ) ) ;
#20728 = ORIENTED_EDGE ( 'NONE', *, *, #13055, .F. ) ;
#20729 = CARTESIAN_POINT ( 'NONE',  ( 14.11792989500000139, -6.227520601336999917, -9.073701378510998339 ) ) ;
#20730 = CARTESIAN_POINT ( 'NONE',  ( -6.130190774865132752, 15.95791884716732767, 1.063281737135261418 ) ) ;
#20731 = CARTESIAN_POINT ( 'NONE',  ( -2.104626470933999904, 25.91506359723999964, -1.289728978252000058 ) ) ;
#20732 = VERTEX_POINT ( 'NONE', #3325 ) ;
#20733 = ORIENTED_EDGE ( 'NONE', *, *, #21850, .T. ) ;
#20734 = CARTESIAN_POINT ( 'NONE',  ( -14.00000000000000000, 3.582449869577975399, -8.571500952496775128 ) ) ;
#20735 = CARTESIAN_POINT ( 'NONE',  ( -9.581549711695000582, -0.05265680612012000467, -15.56874310937000061 ) ) ;
#20736 = CARTESIAN_POINT ( 'NONE',  ( 1.394254956788696598, 6.917606337227010904, -1.084076266210869610 ) ) ;
#20737 = CARTESIAN_POINT ( 'NONE',  ( -9.042815982636001948, 21.50000000000000000, 1.000000000000000000 ) ) ;
#20738 = ORIENTED_EDGE ( 'NONE', *, *, #14134, .T. ) ;
#20739 = CARTESIAN_POINT ( 'NONE',  ( 1.699986747157999911, 9.000014340785000400, 0.8485215224771999187 ) ) ;
#20740 = AXIS2_PLACEMENT_3D ( 'NONE', #20607, #14680, #22072 ) ;
#20741 = CARTESIAN_POINT ( 'NONE',  ( 6.151787191419744616, 14.12035391479590452, 0.2847419465408779216 ) ) ;
#20742 = CARTESIAN_POINT ( 'NONE',  ( 15.42724554293097938, -1.981222823747588402, 10.15954205669230959 ) ) ;
#20743 = VECTOR ( 'NONE', #5010, 1000.000000000000114 ) ;
#20744 = CARTESIAN_POINT ( 'NONE',  ( -14.47223966578000010, 9.858263368903999790, 4.889297467510999695 ) ) ;
#20745 = EDGE_CURVE ( 'NONE', #11746, #1877, #2336, .T. ) ;
#20746 = CARTESIAN_POINT ( 'NONE',  ( -1.869146948832999922, 30.84635783959000221, 0.9105165119439999621 ) ) ;
#20747 = CARTESIAN_POINT ( 'NONE',  ( -13.56430720021000091, -8.266217267278999969, 6.000601104121999541 ) ) ;
#20748 = CARTESIAN_POINT ( 'NONE',  ( 0.1279519981187458300, 29.61131102235037815, 2.157129590390447493 ) ) ;
#20749 = VERTEX_POINT ( 'NONE', #23401 ) ;
#20750 = AXIS2_PLACEMENT_3D ( 'NONE', #20548, #5996, #18843 ) ;
#20751 = CARTESIAN_POINT ( 'NONE',  ( -18.05147222760578174, -1.660822553031731763, 10.32521625223683870 ) ) ;
#20752 = ORIENTED_EDGE ( 'NONE', *, *, #9370, .F. ) ;
#20753 = DIRECTION ( 'NONE',  ( -1.000000000000000000, 0.000000000000000000, 0.000000000000000000 ) ) ;
#20754 = LINE ( 'NONE', #4289, #5778 ) ;
#20755 = EDGE_CURVE ( 'NONE', #6003, #10297, #12283, .T. ) ;
#20756 = AXIS2_PLACEMENT_3D ( 'NONE', #5115, #8980, #12496 ) ;
#20757 = CARTESIAN_POINT ( 'NONE',  ( -12.50000000000000000, -7.500000000000000000, 0.000000000000000000 ) ) ;
#20758 = CARTESIAN_POINT ( 'NONE',  ( 17.14893908531000122, -9.665900270332999256, 3.387665420544000217 ) ) ;
#20759 = ORIENTED_EDGE ( 'NONE', *, *, #17956, .F. ) ;
#20760 = DIRECTION ( 'NONE',  ( 0.000000000000000000, 0.9780930753991020632, -0.2081680471550005351 ) ) ;
#20761 = EDGE_CURVE ( 'NONE', #15280, #11438, #12232, .T. ) ;
#20762 = DIRECTION ( 'NONE',  ( 0.6370702608075069495, 0.000000000000000000, -0.7708057360935083313 ) ) ;
#20763 = ORIENTED_EDGE ( 'NONE', *, *, #12170, .T. ) ;
#20764 = CARTESIAN_POINT ( 'NONE',  ( -12.50000000000000000, 6.606768802097000126, -6.099810110451000966 ) ) ;
#20765 = AXIS2_PLACEMENT_3D ( 'NONE', #2694, #4141, #22776 ) ;
#20766 = CARTESIAN_POINT ( 'NONE',  ( -12.48243343204000055, 6.965111533508000718, -5.686492047758000545 ) ) ;
#20767 = CARTESIAN_POINT ( 'NONE',  ( 3.311115755811001371, 12.13908021832000372, 3.509723945568998360 ) ) ;
#20768 = CARTESIAN_POINT ( 'NONE',  ( -14.00000000000000355, -1.546932818872876814, 9.717798975675457029 ) ) ;
#20769 = B_SPLINE_CURVE_WITH_KNOTS ( 'NONE', 3,
 ( #2901, #7861, #21056, #21181 ),
 .UNSPECIFIED., .F., .F.,
 ( 4, 4 ),
 ( 0.2436176585163755404, 0.2478303497282951795 ),
 .UNSPECIFIED. ) ;
#20770 = VECTOR ( 'NONE', #3756, 1000.000000000000000 ) ;
#20771 = CARTESIAN_POINT ( 'NONE',  ( -22.45768008457000064, -0.6428547435799999432, 9.603249762923001143 ) ) ;
#20772 = ADVANCED_FACE ( 'NONE', ( #14446 ), #8767, .T. ) ;
#20773 = CARTESIAN_POINT ( 'NONE',  ( 19.26374770046332330, 5.632616517831162462, -7.329538123794997695 ) ) ;
#20774 = CARTESIAN_POINT ( 'NONE',  ( -9.031350480845023345E-06, 28.86929942113680170, 2.273237782549102803 ) ) ;
#20775 = CARTESIAN_POINT ( 'NONE',  ( 2.500000000000000000, 18.50000000000000000, 0.000000000000000000 ) ) ;
#20776 = CARTESIAN_POINT ( 'NONE',  ( 5.274219629769681283, 13.82795425090464114, -4.206144534439919980 ) ) ;
#20777 = CARTESIAN_POINT ( 'NONE',  ( 2.184465970885644648, 27.90086340285666822, -1.259047450927249345 ) ) ;
#20778 = CARTESIAN_POINT ( 'NONE',  ( 1.105833872631340364, 30.47227404555147956, 1.856455373682658117 ) ) ;
#20779 = VERTEX_POINT ( 'NONE', #12410 ) ;
#20780 = CARTESIAN_POINT ( 'NONE',  ( -17.80824577250665897, 2.389424319302919653, -8.890643215737140892 ) ) ;
#20781 = CARTESIAN_POINT ( 'NONE',  ( 19.78796100793000079, 4.592772578639999992, 8.629704802492000226 ) ) ;
#20782 = CARTESIAN_POINT ( 'NONE',  ( 0.2655874759832465570, 12.80453501645971137, -6.661713502021730626 ) ) ;
#20783 = CARTESIAN_POINT ( 'NONE',  ( 1.099193499486128323, 29.93562577624026488, 3.984182490697167900 ) ) ;
#20784 = CARTESIAN_POINT ( 'NONE',  ( -22.03664591665549821, 10.47998752884019957, -2.062401532638290735 ) ) ;
#20785 = CARTESIAN_POINT ( 'NONE',  ( -2.383523424258999768, 28.38946440325999987, -0.6219987658658000518 ) ) ;
#20786 = EDGE_CURVE ( 'NONE', #18240, #13009, #1009, .T. ) ;
#20787 = AXIS2_PLACEMENT_3D ( 'NONE', #5715, #11652, #7771 ) ;
#20788 = DIRECTION ( 'NONE',  ( 0.000000000000000000, -1.000000000000000000, 0.000000000000000000 ) ) ;
#20789 = ORIENTED_EDGE ( 'NONE', *, *, #14605, .T. ) ;
#20790 = CARTESIAN_POINT ( 'NONE',  ( -18.41005308736142965, 10.25486752108468202, -2.049228009546027351 ) ) ;
#20791 = CARTESIAN_POINT ( 'NONE',  ( 24.43449445986659896, 11.92557563953692856, 4.344297082815015365 ) ) ;
#20792 = VECTOR ( 'NONE', #22483, 1000.000000000000227 ) ;
#20793 = DIRECTION ( 'NONE',  ( 0.000000000000000000, -1.000000000000000000, 0.000000000000000000 ) ) ;
#20794 = CARTESIAN_POINT ( 'NONE',  ( -10.90000000000000036, -10.50000000000000000, -1.712918112906000235E-09 ) ) ;
#20795 = ORIENTED_EDGE ( 'NONE', *, *, #11594, .F. ) ;
#20796 = CARTESIAN_POINT ( 'NONE',  ( 17.10962270046334055, -4.588261632613977348, -7.960449803099588273 ) ) ;
#20797 = CARTESIAN_POINT ( 'NONE',  ( 15.09131424931000076, 4.764171260128000185, 9.577928620034999341 ) ) ;
#20798 = EDGE_CURVE ( 'NONE', #11418, #23198, #19598, .T. ) ;
#20799 = DIRECTION ( 'NONE',  ( 0.000000000000000000, 0.000000000000000000, -1.000000000000000000 ) ) ;
#20800 = CARTESIAN_POINT ( 'NONE',  ( 22.68304166666665367, 7.399526017309272063, -5.686719956180886548 ) ) ;
#20801 = EDGE_CURVE ( 'NONE', #12095, #21674, #17655, .T. ) ;
#20802 = CARTESIAN_POINT ( 'NONE',  ( 14.92176537305999950, 8.069302409968999612, -7.172646714567000537 ) ) ;
#20803 = DIRECTION ( 'NONE',  ( 0.000000000000000000, 1.000000000000000000, 0.000000000000000000 ) ) ;
#20804 = CARTESIAN_POINT ( 'NONE',  ( -8.099999999999999645, 9.651424765286998664, 1.370595831274000043E-09 ) ) ;
#20805 = CARTESIAN_POINT ( 'NONE',  ( 24.38524151196000034, 9.842852006268000054, -3.081908802582999485 ) ) ;
#20806 = PRODUCT ( 'MAS-673 Main Body', 'MAS-673 Main Body', '', ( #18011 ) ) ;
#20807 = CARTESIAN_POINT ( 'NONE',  ( 2.649085689637681540, 29.97444252552741872, 3.089351817498231068 ) ) ;
#20808 = VERTEX_POINT ( 'NONE', #2190 ) ;
#20809 = CARTESIAN_POINT ( 'NONE',  ( 11.85282401169000188, -8.499855654764999713, -2.882903103473000161 ) ) ;
#20810 = CARTESIAN_POINT ( 'NONE',  ( -1.948889566018999986, 27.36500240009999985, 2.108296854627000005 ) ) ;
#20811 = CARTESIAN_POINT ( 'NONE',  ( -4.719941065002002389, 12.37770080416001051, 1.073222396542000023 ) ) ;
#20812 = CARTESIAN_POINT ( 'NONE',  ( 24.39856360185587647, -9.628104977245440566, -2.325364009612112870 ) ) ;
#20813 = CARTESIAN_POINT ( 'NONE',  ( -21.28778663430999885, -8.840331526475999624, 6.688932671969999078 ) ) ;
#20814 = ORIENTED_EDGE ( 'NONE', *, *, #2750, .F. ) ;
#20815 = ADVANCED_FACE ( 'NONE', ( #7521 ), #4108, .T. ) ;
#20816 = EDGE_CURVE ( 'NONE', #6675, #14207, #1793, .T. ) ;
#20817 = CARTESIAN_POINT ( 'NONE',  ( 1.699986222664000124, 9.100024384209000061, 1.053575639828000066 ) ) ;
#20818 = ORIENTED_EDGE ( 'NONE', *, *, #9402, .F. ) ;
#20819 = B_SPLINE_CURVE_WITH_KNOTS ( 'NONE', 3,
 ( #20177, #22213, #10860, #20412, #3938, #1647, #1765, #23797, #14597, #23917 ),
 .UNSPECIFIED., .F., .F.,
 ( 4, 2, 2, 2, 4 ),
 ( 0.000000000000000000, 0.2500000000000001110, 0.5000000000000001110, 0.7500000000000001110, 1.000000000000000000 ),
 .UNSPECIFIED. ) ;
#20820 = CARTESIAN_POINT ( 'NONE',  ( -3.000000000000000000, 21.89999999999999858, 0.000000000000000000 ) ) ;
#20821 = CARTESIAN_POINT ( 'NONE',  ( -1.857441216906001724, 12.79832155229998314, 6.826339096581000021 ) ) ;
#20822 = CIRCLE ( 'NONE', #8455, 2.000000000000000000 ) ;
#20823 = CARTESIAN_POINT ( 'NONE',  ( -1.304206744018095554, 6.901791827019449599, 1.169639274656592898 ) ) ;
#20824 = CARTESIAN_POINT ( 'NONE',  ( 13.99443924931000005, -9.599271117524001085, -4.655318192544999789 ) ) ;
#20825 = CARTESIAN_POINT ( 'NONE',  ( -18.07393293677000301, 10.37468091520999991, 3.263143967163999903 ) ) ;
#20826 = CARTESIAN_POINT ( 'NONE',  ( 15.67012625730999886, 7.503068644359999873, -5.298384255253999697 ) ) ;
#20827 = DIRECTION ( 'NONE',  ( -1.000000000000000000, 0.000000000000000000, 0.000000000000000000 ) ) ;
#20828 = AXIS2_PLACEMENT_3D ( 'NONE', #1779, #1661, #10875 ) ;
#20829 = ORIENTED_EDGE ( 'NONE', *, *, #1977, .T. ) ;
#20830 = CARTESIAN_POINT ( 'NONE',  ( 1.146872940636000093, 31.00466803249999970, -2.470645430041999990 ) ) ;
#20831 = CARTESIAN_POINT ( 'NONE',  ( -0.9534504523828000178, 24.43033993841000040, 2.338684930832999775 ) ) ;
#20832 = AXIS2_PLACEMENT_3D ( 'NONE', #13025, #7218, #7452 ) ;
#20833 = CARTESIAN_POINT ( 'NONE',  ( 13.50000000000000000, 2.048741218006000064, 10.08990150394999930 ) ) ;
#20834 = AXIS2_PLACEMENT_3D ( 'NONE', #12294, #18107, #8780 ) ;
#20835 = ORIENTED_EDGE ( 'NONE', *, *, #1992, .F. ) ;
#20836 = CARTESIAN_POINT ( 'NONE',  ( 0.5469854966064994217, 13.20286669322999806, -6.078858689229004852 ) ) ;
#20837 = CARTESIAN_POINT ( 'NONE',  ( 19.24289560999000059, -4.617872442541000488, 10.17084159971000012 ) ) ;
#20838 = CARTESIAN_POINT ( 'NONE',  ( 0.7149603813832000609, 30.34065304942999575, -2.650948342028000226 ) ) ;
#20839 = CARTESIAN_POINT ( 'NONE',  ( 14.40622728660040508, -4.514104690157912714, 7.833270047916061962 ) ) ;
#20840 = CARTESIAN_POINT ( 'NONE',  ( -1.779764907139927077, 26.49975665830813298, 1.755621799651315262 ) ) ;
#20841 = DIRECTION ( 'NONE',  ( 1.000000000000000000, 0.000000000000000000, 0.000000000000000000 ) ) ;
#20842 = AXIS2_PLACEMENT_3D ( 'NONE', #10276, #4715, #14028 ) ;
#20843 = CARTESIAN_POINT ( 'NONE',  ( 0.000000000000000000, -9.000000000000000000, 0.000000000000000000 ) ) ;
#20844 = CARTESIAN_POINT ( 'NONE',  ( 23.99062354302999722, -13.93375672974000068, -0.8660254037843999608 ) ) ;
#20845 = EDGE_LOOP ( 'NONE', ( #21062, #22956, #20200 ) ) ;
#20846 = DIRECTION ( 'NONE',  ( 0.000000000000000000, 0.5009995559142040866, -0.8654475402783060600 ) ) ;
#20847 = EDGE_LOOP ( 'NONE', ( #13727, #1079, #4508, #9755, #17095, #20447 ) ) ;
#20848 = AXIS2_PLACEMENT_3D ( 'NONE', #15612, #10434, #9934 ) ;
#20849 = FACE_OUTER_BOUND ( 'NONE', #6871, .T. ) ;
#20851 = CARTESIAN_POINT ( 'NONE',  ( -1.999537075602261016, 23.75013256832107444, -0.9022053864054707661 ) ) ;
#20850 = DIRECTION ( 'NONE',  ( 1.000000000000000000, 0.000000000000000000, 0.000000000000000000 ) ) ;
#20852 = CARTESIAN_POINT ( 'NONE',  ( 1.556904262685800289, 24.71889605908289056, 1.535089544408534179 ) ) ;
#20853 = AXIS2_PLACEMENT_3D ( 'NONE', #20539, #2123, #4303 ) ;
#20854 = CARTESIAN_POINT ( 'NONE',  ( -14.25243324638999809, 13.93375672974000068, -0.8660254037843999608 ) ) ;
#20855 = CARTESIAN_POINT ( 'NONE',  ( -6.990117763008002250, 15.33795737441000995, -1.812023283503998883 ) ) ;
#20856 = PRODUCT_RELATED_PRODUCT_CATEGORY ( 'part', '', ( #11128 ) ) ;
#20857 = CARTESIAN_POINT ( 'NONE',  ( 2.621867217767999581, 25.34669433610000056, 0.5899383557787000187 ) ) ;
#20858 = ORIENTED_EDGE ( 'NONE', *, *, #17493, .F. ) ;
#20859 = ORIENTED_EDGE ( 'NONE', *, *, #9231, .T. ) ;
#20860 = CARTESIAN_POINT ( 'NONE',  ( -24.37124162824695617, 9.546779961769933820, -8.464497487737872916 ) ) ;
#20861 = CIRCLE ( 'NONE', #1529, 3.000000000000001332 ) ;
#20862 = DIRECTION ( 'NONE',  ( 1.000000000000000000, 0.000000000000000000, 0.000000000000000000 ) ) ;
#20863 = CARTESIAN_POINT ( 'NONE',  ( -24.16119556689903902, -8.771053125573958553, -9.807567373703745872 ) ) ;
#20864 = VERTEX_POINT ( 'NONE', #3902 ) ;
#20865 = CARTESIAN_POINT ( 'NONE',  ( -24.13073565549000321, -9.140001432355999711, -4.665568137828999262 ) ) ;
#20866 = CARTESIAN_POINT ( 'NONE',  ( -24.11803009771418616, 8.641091274403159161, 10.03259869781534519 ) ) ;
#20867 = CARTESIAN_POINT ( 'NONE',  ( 6.141065191050296690, 14.19649558781827103, 0.04858547980339427558 ) ) ;
#20868 = CARTESIAN_POINT ( 'NONE',  ( 15.65124655084372840, -8.589975589872866024, 5.797750052853028357 ) ) ;
#20869 = CARTESIAN_POINT ( 'NONE',  ( -15.63475771655999758, -5.016338890459000055, -9.829993491887998758 ) ) ;
#20870 = CIRCLE ( 'NONE', #23587, 2.399999999999999911 ) ;
#20871 = CARTESIAN_POINT ( 'NONE',  ( -2.008526492215999770, 30.87968012902000225, 0.9784123912684001834 ) ) ;
#20872 = DIRECTION ( 'NONE',  ( 1.000000000000000000, 0.000000000000000000, 0.000000000000000000 ) ) ;
#20873 = TOROIDAL_SURFACE ( 'NONE', #1155, 7.200000000000000178, 0.1000000000000000056 ) ;
#20874 = CARTESIAN_POINT ( 'NONE',  ( -15.23010806520000138, -8.044096712135001326, -7.201187562783000651 ) ) ;
#20875 = CARTESIAN_POINT ( 'NONE',  ( 0.2157408166878850564, 29.61644974637328431, 2.149169616069145583 ) ) ;
#20876 = VERTEX_POINT ( 'NONE', #7768 ) ;
#20877 = CARTESIAN_POINT ( 'NONE',  ( -0.5326254371206000648, 23.42133201074999960, -2.045335842707999952 ) ) ;
#20878 = CARTESIAN_POINT ( 'NONE',  ( -18.48555983533165303, 10.20055682982866685, 2.347179025034034971 ) ) ;
#20879 = ORIENTED_EDGE ( 'NONE', *, *, #13937, .T. ) ;
#20880 = CARTESIAN_POINT ( 'NONE',  ( -1.823227943893884984, 24.59979839667439805, -1.434329759635685209 ) ) ;
#20881 = CARTESIAN_POINT ( 'NONE',  ( -4.860485347078998153, 13.74172132047000794, 4.702795991816000942 ) ) ;
#20882 = CARTESIAN_POINT ( 'NONE',  ( 1.236794719700695211, 24.50000548481460427, 2.172625763342098004 ) ) ;
#20883 = EDGE_CURVE ( 'NONE', #17924, #23795, #18324, .T. ) ;
#20884 = CARTESIAN_POINT ( 'NONE',  ( 14.05125142131000082, 6.790538403688000102, -6.859017754185999571 ) ) ;
#20885 = VERTEX_POINT ( 'NONE', #5595 ) ;
#20886 = CARTESIAN_POINT ( 'NONE',  ( -6.017198780830001148, 15.84372863255997821, -1.061654000538000409 ) ) ;
#20887 = CARTESIAN_POINT ( 'NONE',  ( -4.850000000102999920, 12.44999864901999942, -1.732907964652000048E-09 ) ) ;
#20888 = ORIENTED_EDGE ( 'NONE', *, *, #23767, .F. ) ;
#20889 = DIRECTION ( 'NONE',  ( 1.000000000000000000, 0.000000000000000000, 0.000000000000000000 ) ) ;
#20890 = B_SPLINE_CURVE_WITH_KNOTS ( 'NONE', 3,
 ( #16937, #1699, #5804, #9204, #15109, #18645, #18406, #5545, #7379, #11268, #5914, #2051, #20122, #9442, #18298, #220, #7617, #573 ),
 .UNSPECIFIED., .F., .F.,
 ( 4, 2, 2, 2, 2, 2, 2, 2, 4 ),
 ( 0.000000000000000000, 0.1250000000000000000, 0.2500000000000000000, 0.3750000000000000000, 0.5000000000000000000, 0.6250000000000000000, 0.7500000000000000000, 0.8750000000000000000, 1.000000000000000000 ),
 .UNSPECIFIED. ) ;
#20891 = CARTESIAN_POINT ( 'NONE',  ( 21.66266666666665941, -4.646869946770923576, 8.062640237677072719 ) ) ;
#20892 = CARTESIAN_POINT ( 'NONE',  ( -3.580425678944999301, 12.20479645082998843, 3.123592402036998283 ) ) ;
#20893 = CARTESIAN_POINT ( 'NONE',  ( 4.835083642289389694, 12.44448910615697912, 0.3758261001295359338 ) ) ;
#20894 = CARTESIAN_POINT ( 'NONE',  ( 18.39048037518193368, 8.950322807170842054, -5.337459449838163117 ) ) ;
#20895 = CIRCLE ( 'NONE', #1173, 10.65000000000000036 ) ;
#20896 = DIRECTION ( 'NONE',  ( -1.000000000000000000, 0.000000000000000000, 0.000000000000000000 ) ) ;
#20897 = EDGE_CURVE ( 'NONE', #9922, #19778, #15024, .T. ) ;
#20898 = DIRECTION ( 'NONE',  ( 0.000000000000000000, 1.000000000000000000, 0.000000000000000000 ) ) ;
#20899 = CARTESIAN_POINT ( 'NONE',  ( -5.147503733180995411, 15.83089091750001742, -2.717754031361000688 ) ) ;
#20900 = DIRECTION ( 'NONE',  ( 1.000000000000000000, 0.000000000000000000, 0.000000000000000000 ) ) ;
#20901 = CARTESIAN_POINT ( 'NONE',  ( 5.243253597151068313, 14.63899575032571221, 3.172841098946398208 ) ) ;
#20902 = DIRECTION ( 'NONE',  ( 0.000000000000000000, 1.000000000000000000, 0.000000000000000000 ) ) ;
#20903 = CARTESIAN_POINT ( 'NONE',  ( 0.9906019889434464210, 30.46455799699790745, 1.919774432312305823 ) ) ;
#20904 = VERTEX_POINT ( 'NONE', #11294 ) ;
#20905 = CARTESIAN_POINT ( 'NONE',  ( -4.563746053395999702, 28.00000000000000000, 4.080056528100000079 ) ) ;
#20906 = CARTESIAN_POINT ( 'NONE',  ( 2.046202797321268196, 12.94580643705319645, -6.382747573611354142 ) ) ;
#20907 = DIRECTION ( 'NONE',  ( 0.000000000000000000, -1.000000000000000000, 0.000000000000000000 ) ) ;
#20908 = CARTESIAN_POINT ( 'NONE',  ( -19.78743041492825583, 2.646772407754812928, 10.15050686662911872 ) ) ;
#20909 = CARTESIAN_POINT ( 'NONE',  ( 1.683383295848999817, 27.28364211382000093, -1.556103512505999875 ) ) ;
#20910 = CARTESIAN_POINT ( 'NONE',  ( -6.253205914068437288, 26.47872451769842783, 1.076069669024710906 ) ) ;
#20911 = EDGE_LOOP ( 'NONE', ( #14572, #16733, #255, #1790, #10624, #11512 ) ) ;
#20912 = EDGE_CURVE ( 'NONE', #21756, #15925, #1424, .T. ) ;
#20913 = CARTESIAN_POINT ( 'NONE',  ( -17.37733730988356839, -10.13133732267558074, -2.466463703678301478 ) ) ;
#20914 = LINE ( 'NONE', #10013, #22331 ) ;
#20915 = DIRECTION ( 'NONE',  ( 0.000000000000000000, 0.8660254037844288266, -0.5000000000000169864 ) ) ;
#20916 = VECTOR ( 'NONE', #13419, 1000.000000000000114 ) ;
#20917 = DIRECTION ( 'NONE',  ( 0.000000000000000000, 1.000000000000000000, 0.000000000000000000 ) ) ;
#20918 = VERTEX_POINT ( 'NONE', #16969 ) ;
#20919 = CARTESIAN_POINT ( 'NONE',  ( 17.33637270046333612, 2.386020194961869123, -8.878946354107190686 ) ) ;
#20920 = CARTESIAN_POINT ( 'NONE',  ( 16.07850174930999998, -1.960161522604999762, -10.54265994730999978 ) ) ;
#20921 = EDGE_CURVE ( 'NONE', #12884, #12435, #17345, .T. ) ;
#20922 = DIRECTION ( 'NONE',  ( 0.000000000000000000, 0.000000000000000000, -1.000000000000000000 ) ) ;
#20923 = CARTESIAN_POINT ( 'NONE',  ( 0.000000000000000000, 7.216878364870000340, 12.50000000000000000 ) ) ;
#20924 = CARTESIAN_POINT ( 'NONE',  ( 13.70301537305999950, 2.512834476447000309, 10.46490100832000003 ) ) ;
#20925 = CARTESIAN_POINT ( 'NONE',  ( 13.50000000000000178, -4.872488826576057974, -7.717741468829464324 ) ) ;
#20926 = CARTESIAN_POINT ( 'NONE',  ( 20.49016126455000020, 3.425869769563000045, -9.615571166989999696 ) ) ;
#20927 = CARTESIAN_POINT ( 'NONE',  ( -2.500000000000001332, 26.61184640831621806, -0.4388476615849645768 ) ) ;
#20928 = ORIENTED_EDGE ( 'NONE', *, *, #14256, .F. ) ;
#20929 = CARTESIAN_POINT ( 'NONE',  ( 3.000000000000000000, 22.00000000000000000, 0.000000000000000000 ) ) ;
#20930 = CARTESIAN_POINT ( 'NONE',  ( 1.652809762273000027, 26.86956776951999970, -2.096579189799000265 ) ) ;
#20931 = CARTESIAN_POINT ( 'NONE',  ( -3.577956154687000900, 12.12797091520000592, 3.101079032933002466 ) ) ;
#20932 = EDGE_CURVE ( 'NONE', #23649, #19406, #5480, .T. ) ;
#20933 = CARTESIAN_POINT ( 'NONE',  ( 24.19085492956958561, -9.549256642876626344, 0.0002501093553063627687 ) ) ;
#20934 = CARTESIAN_POINT ( 'NONE',  ( -20.59898550229000236, 6.916942397327000336, -8.639163530769000232 ) ) ;
#20935 = EDGE_LOOP ( 'NONE', ( #6964, #21524, #2444, #1768, #13417 ) ) ;
#20936 = CARTESIAN_POINT ( 'NONE',  ( -5.529771451991000397, 1.198997689148999791E-14, -12.68487026514986837 ) ) ;
#20937 = ORIENTED_EDGE ( 'NONE', *, *, #9850, .F. ) ;
#20938 = ADVANCED_FACE ( 'NONE', ( #7405 ), #16872, .T. ) ;
#20939 = CARTESIAN_POINT ( 'NONE',  ( -20.25016455292000117, -8.657612072530000091, 3.085311466348000131 ) ) ;
#20940 = FACE_OUTER_BOUND ( 'NONE', #8718, .T. ) ;
#20941 = CARTESIAN_POINT ( 'NONE',  ( 24.25008227645999881, 0.000000000000000000, 0.000000000000000000 ) ) ;
#20942 = EDGE_CURVE ( 'NONE', #4204, #19823, #7824, .T. ) ;
#20943 = CARTESIAN_POINT ( 'NONE',  ( -0.4973687615736275824, 6.795906696827745286, 1.678020886483821972 ) ) ;
#20944 = CARTESIAN_POINT ( 'NONE',  ( 13.33631424930999998, 2.709556187140999661, 10.30084784107000040 ) ) ;
#20945 = CARTESIAN_POINT ( 'NONE',  ( -17.26141154489999963, -10.85036612823000013, 0.2443279951607999767 ) ) ;
#20946 = CARTESIAN_POINT ( 'NONE',  ( 11.94075125730999964, 5.167059442038000050, -7.475232529384999047 ) ) ;
#20947 = CARTESIAN_POINT ( 'NONE',  ( 24.36165043081783921, 12.41271798542465810, -3.500541789220333211 ) ) ;
#20948 = ORIENTED_EDGE ( 'NONE', *, *, #20942, .T. ) ;
#20949 = EDGE_CURVE ( 'NONE', #93, #21190, #7514, .T. ) ;
#20950 = CARTESIAN_POINT ( 'NONE',  ( 1.699553337878000114, 29.94579250490999911, 2.128570997566999967 ) ) ;
#20951 = EDGE_CURVE ( 'NONE', #12236, #10709, #3211, .T. ) ;
#20952 = CARTESIAN_POINT ( 'NONE',  ( 2.429900969743000072, 25.49769184508999942, -0.3508820655058000337 ) ) ;
#20953 = CARTESIAN_POINT ( 'NONE',  ( 14.16427405790947525, -8.883215205009282300, -5.323156792243073809 ) ) ;
#20954 = CARTESIAN_POINT ( 'NONE',  ( 5.223518823337998995, 13.88591009669999643, -3.771757984836998201 ) ) ;
#20955 = CARTESIAN_POINT ( 'NONE',  ( -23.74465998031000069, 13.93375672974000068, -0.8660254037843999608 ) ) ;
#20956 = FACE_OUTER_BOUND ( 'NONE', #14204, .T. ) ;
#20957 = CARTESIAN_POINT ( 'NONE',  ( 12.52688711657000020, 6.216878364870000340, 12.50000000000000000 ) ) ;
#20958 = PLANE ( 'NONE',  #6920 ) ;
#20959 = DIRECTION ( 'NONE',  ( 0.000000000000000000, 1.000000000000000000, 0.000000000000000000 ) ) ;
#20960 = DIRECTION ( 'NONE',  ( 0.000000000000000000, -1.000000000000000000, 0.000000000000000000 ) ) ;
#20961 = CARTESIAN_POINT ( 'NONE',  ( 23.99895687519799381, 13.93375672974000068, -0.3849913042976704780 ) ) ;
#20962 = ORIENTED_EDGE ( 'NONE', *, *, #22865, .F. ) ;
#20963 = CARTESIAN_POINT ( 'NONE',  ( 4.749995115181361527, 12.55003697659937778, -0.6285192019201937264 ) ) ;
#20964 = VERTEX_POINT ( 'NONE', #19138 ) ;
#20965 = CARTESIAN_POINT ( 'NONE',  ( 23.99062354302999722, 7.716878364870000340, 11.63397459621999985 ) ) ;
#20967 = CARTESIAN_POINT ( 'NONE',  ( -2.133777946215778432, 23.65390751601632857, 0.3359879145818772117 ) ) ;
#20966 = CARTESIAN_POINT ( 'NONE',  ( -2.212704257922113005, 11.69046487145196878, 4.282078202130872313 ) ) ;
#20968 = CARTESIAN_POINT ( 'NONE',  ( -1.839173991642404582, 30.00000000000000711, -3.556954554355652220 ) ) ;
#20969 = CARTESIAN_POINT ( 'NONE',  ( 13.68936949739000042, -0.4386406477174999985, 10.98417168335999961 ) ) ;
#20970 = CARTESIAN_POINT ( 'NONE',  ( -10.04281598263999875, 16.40330333352000025, 0.9999999999983999466 ) ) ;
#20971 = DIRECTION ( 'NONE',  ( 1.000000000000000000, 0.000000000000000000, 0.000000000000000000 ) ) ;
#20972 = ORIENTED_EDGE ( 'NONE', *, *, #19914, .F. ) ;
#20973 = EDGE_LOOP ( 'NONE', ( #19377, #14739 ) ) ;
#20974 = CARTESIAN_POINT ( 'NONE',  ( -14.00000000000000355, -2.579277104765260287, -9.307187374249766165 ) ) ;
#20975 = DIRECTION ( 'NONE',  ( -1.000000000000000000, 0.000000000000000000, 0.000000000000000000 ) ) ;
#20976 = CARTESIAN_POINT ( 'NONE',  ( 2.000000000000000000, 18.10000000000000142, 0.000000000000000000 ) ) ;
#20977 = ORIENTED_EDGE ( 'NONE', *, *, #9399, .T. ) ;
#20978 = EDGE_CURVE ( 'NONE', #15392, #19135, #13005, .T. ) ;
#20979 = CARTESIAN_POINT ( 'NONE',  ( -22.00181313460999988, -7.290803318660999288, -6.369760926427000314 ) ) ;
#20980 = CARTESIAN_POINT ( 'NONE',  ( 1.712415232174588686, 12.94871783748642535, -1.057129568949859877 ) ) ;
#20981 = CARTESIAN_POINT ( 'NONE',  ( 0.000000000000000000, 20.04999987253368943, -2.704938617610999654E-14 ) ) ;
#20982 = CARTESIAN_POINT ( 'NONE',  ( 15.83035365568370345, -10.35462237868133251, -0.2935575748633351134 ) ) ;
#20983 = CARTESIAN_POINT ( 'NONE',  ( -15.48813611968000004, -5.014512979174000407, -9.826416270666999964 ) ) ;
#20984 = CARTESIAN_POINT ( 'NONE',  ( -4.649999849441000421, 17.00000015055400127, 6.648422636708999828E-08 ) ) ;
#20985 = CARTESIAN_POINT ( 'NONE',  ( -21.20489941501549680, -10.23248319439458598, -2.462552185894037571 ) ) ;
#20986 = AXIS2_PLACEMENT_3D ( 'NONE', #13946, #21341, #20862 ) ;
#20987 = CARTESIAN_POINT ( 'NONE',  ( -12.75178580833000019, 5.886008164689000566, -8.319303600761999817 ) ) ;
#20988 = CARTESIAN_POINT ( 'NONE',  ( -1.790837194179027314, 29.47926921055185545, 1.208204829431328342 ) ) ;
#20989 = EDGE_LOOP ( 'NONE', ( #4257, #22661, #13455, #18786 ) ) ;
#20990 = CARTESIAN_POINT ( 'NONE',  ( -1.273908836082999985, 23.46786385441999911, -1.776248845517000019 ) ) ;
#20991 = CARTESIAN_POINT ( 'NONE',  ( -18.74601239996717084, 8.305110545182456505, -6.624969937855211377 ) ) ;
#20992 = ORIENTED_EDGE ( 'NONE', *, *, #9098, .F. ) ;
#20993 = CARTESIAN_POINT ( 'NONE',  ( -1.989420752042081908, 24.61064990806593045, -1.172145431141076388 ) ) ;
#20994 = CARTESIAN_POINT ( 'NONE',  ( 6.258925775870999075, 13.70565998269001007, -0.4762665460848001797 ) ) ;
#20995 = CARTESIAN_POINT ( 'NONE',  ( -9.042815982636001948, 21.50000000000000000, -1.000000000000000000 ) ) ;
#20996 = CARTESIAN_POINT ( 'NONE',  ( -19.61634587121332984, 8.935932136875853971, -2.401334698577377136 ) ) ;
#20997 = CARTESIAN_POINT ( 'NONE',  ( 17.36831408530999710, -9.345903658884999743, -4.204539402675000481 ) ) ;
#20998 = VERTEX_POINT ( 'NONE', #19269 ) ;
#20999 = VECTOR ( 'NONE', #14770, 1000.000000000000114 ) ;
#21000 = CYLINDRICAL_SURFACE ( 'NONE', #17183, 4.750000000000000000 ) ;
#21001 = DIRECTION ( 'NONE',  ( 0.000000000000000000, -0.8660254037844288266, -0.5000000000000169864 ) ) ;
#21002 = FACE_OUTER_BOUND ( 'NONE', #20032, .T. ) ;
#21003 = ORIENTED_EDGE ( 'NONE', *, *, #14267, .F. ) ;
#21004 = CARTESIAN_POINT ( 'NONE',  ( -12.50000000000000000, 6.907686671057999384, -5.757541812536000059 ) ) ;
#21005 = CARTESIAN_POINT ( 'NONE',  ( 21.20916666666666828, 8.052471370503557324, 4.641008978248494010 ) ) ;
#21006 = DIRECTION ( 'NONE',  ( 0.000000000000000000, -1.000000000000000000, 0.000000000000000000 ) ) ;
#21007 = CARTESIAN_POINT ( 'NONE',  ( 3.999999999999999112, 26.42936170367562809, 1.090349405812182315 ) ) ;
#21008 = CARTESIAN_POINT ( 'NONE',  ( 17.66429342642312506, -10.35204213498203529, -1.010235597007892450 ) ) ;
#21009 = DIRECTION ( 'NONE',  ( 0.000000000000000000, -1.000000000000000000, 0.000000000000000000 ) ) ;
#21010 = CARTESIAN_POINT ( 'NONE',  ( -14.44633174692025257, -9.404057468159601640, 8.711677720893282739 ) ) ;
#21011 = CARTESIAN_POINT ( 'NONE',  ( 20.05093419402000166, 9.971126252470000395, -5.084926271798999586 ) ) ;
#21012 = CARTESIAN_POINT ( 'NONE',  ( -24.50000000000000000, -9.995791495354000133, -2.484784171996999635 ) ) ;
#21013 = CARTESIAN_POINT ( 'NONE',  ( -0.3272492347489394104, 28.85086340285666751, -2.499999999999999112 ) ) ;
#21014 = CARTESIAN_POINT ( 'NONE',  ( 1.800000000000000044, 13.00000000000000000, -1.081665382638999917 ) ) ;
#21015 = EDGE_CURVE ( 'NONE', #5364, #6975, #14180, .T. ) ;
#21016 = CARTESIAN_POINT ( 'NONE',  ( -0.5448911592932419445, 30.37147015205572487, 2.090315897457275085 ) ) ;
#21017 = VERTEX_POINT ( 'NONE', #20965 ) ;
#21018 = CARTESIAN_POINT ( 'NONE',  ( 21.57978114040000150, 10.23905130607999858, 1.583883726447000040 ) ) ;
#21019 = CARTESIAN_POINT ( 'NONE',  ( 1.988887572331500264, 12.93803022255735513, -6.398493247991286381 ) ) ;
#21020 = DIRECTION ( 'NONE',  ( 1.000000000000000000, 0.000000000000000000, 0.000000000000000000 ) ) ;
#21021 = CARTESIAN_POINT ( 'NONE',  ( 1.014287269782000012, 28.68196440326000030, 1.990650851275000299 ) ) ;
#21022 = VECTOR ( 'NONE', #17007, 1000.000000000000114 ) ;
#21023 = CARTESIAN_POINT ( 'NONE',  ( 12.49102043339000012, -6.966941063182999549, 12.06695109921999887 ) ) ;
#21024 = EDGE_LOOP ( 'NONE', ( #4716, #22897, #6729, #20937 ) ) ;
#21025 = CARTESIAN_POINT ( 'NONE',  ( -18.63334298519549037, 5.912611358794215732, -8.628805914905690599 ) ) ;
#21026 = CARTESIAN_POINT ( 'NONE',  ( 4.649999849441000421, 14.99999984944626696, -6.648422669304000250E-08 ) ) ;
#21027 = CARTESIAN_POINT ( 'NONE',  ( 2.153767644672030634, 28.01336032157206546, 0.2789828094273491543 ) ) ;
#21028 = ORIENTED_EDGE ( 'NONE', *, *, #20575, .F. ) ;
#21029 = ORIENTED_EDGE ( 'NONE', *, *, #1522, .F. ) ;
#21030 = DIRECTION ( 'NONE',  ( -1.000000000000000000, 0.000000000000000000, 0.000000000000000000 ) ) ;
#21031 = CARTESIAN_POINT ( 'NONE',  ( 15.42037674930999991, -6.716928621565999791, 8.336789182003000676 ) ) ;
#21032 = AXIS2_PLACEMENT_3D ( 'NONE', #23741, #16464, #23632 ) ;
#21033 = CARTESIAN_POINT ( 'NONE',  ( -24.75634994828000046, -3.427561506178000261, -9.776571129776000291 ) ) ;
#21034 = FACE_OUTER_BOUND ( 'NONE', #1694, .T. ) ;
#21035 = CARTESIAN_POINT ( 'NONE',  ( 20.15099999999999980, -9.188396088570998543, 0.000000000000000000 ) ) ;
#21036 = CARTESIAN_POINT ( 'NONE',  ( 17.49562451746000136, 9.785307064097999330, 0.2529327338658999835 ) ) ;
#21037 = DIRECTION ( 'NONE',  ( 0.000000000000000000, 0.000000000000000000, -1.000000000000000000 ) ) ;
#21038 = DIRECTION ( 'NONE',  ( 0.000000000000000000, 0.000000000000000000, 1.000000000000000000 ) ) ;
#21039 = CARTESIAN_POINT ( 'NONE',  ( 24.83359518631000284, 9.330707640295999639, 2.986814357572999956 ) ) ;
#21040 = ADVANCED_FACE ( 'NONE', ( #20849 ), #21142, .T. ) ;
#21041 = CARTESIAN_POINT ( 'NONE',  ( 4.000000000000000000, 24.50000000000000000, 0.000000000000000000 ) ) ;
#21042 = ORIENTED_EDGE ( 'NONE', *, *, #5432, .F. ) ;
#21043 = VECTOR ( 'NONE', #13702, 1000.000000000000114 ) ;
#21044 = AXIS2_PLACEMENT_3D ( 'NONE', #4319, #20793, #19083 ) ;
#21045 = CARTESIAN_POINT ( 'NONE',  ( 1.498680770896810621, 13.80134043704015134, 5.938834979248682977 ) ) ;
#21046 = CARTESIAN_POINT ( 'NONE',  ( 0.5071914623445000769, 28.87663313894999817, 2.254114612530000006 ) ) ;
#21047 = CARTESIAN_POINT ( 'NONE',  ( 2.856683780965000974, 11.85702083262999551, 3.848598579512004125 ) ) ;
#21048 = CARTESIAN_POINT ( 'NONE',  ( 1.853950820529611576, 28.93531059620830703, 1.108663733423250086 ) ) ;
#21049 = CARTESIAN_POINT ( 'NONE',  ( -24.29530845835000008, -0.7740144453498000177, -11.14062775012999928 ) ) ;
#21050 = CYLINDRICAL_SURFACE ( 'NONE', #5376, 7.500000000000000000 ) ;
#21051 = ORIENTED_EDGE ( 'NONE', *, *, #19457, .T. ) ;
#21052 = CARTESIAN_POINT ( 'NONE',  ( 15.37120603379664452, -2.373054804797890771, -8.829731701983224212 ) ) ;
#21053 = CARTESIAN_POINT ( 'NONE',  ( 0.000000000000000000, 17.00000000000000000, 0.000000000000000000 ) ) ;
#21054 = EDGE_CURVE ( 'NONE', #2076, #10478, #6185, .T. ) ;
#21055 = CARTESIAN_POINT ( 'NONE',  ( 2.032271969870999673, 13.38796172288000008, 5.759841364760997173 ) ) ;
#21056 = CARTESIAN_POINT ( 'NONE',  ( -1.787520374624578690, 26.49857044772972969, 1.747825089855130187 ) ) ;
#21057 = CYLINDRICAL_SURFACE ( 'NONE', #16919, 3.000000000000000000 ) ;
#21058 = CARTESIAN_POINT ( 'NONE',  ( -19.29271502458999876, -7.174960688273000819, 7.031698840148000507 ) ) ;
#21059 = CARTESIAN_POINT ( 'NONE',  ( 11.72137625731000021, -1.402369408125999861, -8.972525410429000203 ) ) ;
#21060 = EDGE_CURVE ( 'NONE', #19402, #14961, #9821, .T. ) ;
#21061 = CARTESIAN_POINT ( 'NONE',  ( 19.02704979327631563, -1.056774037771824659, 10.41726730992272287 ) ) ;
#21062 = ORIENTED_EDGE ( 'NONE', *, *, #23608, .F. ) ;
#21063 = CARTESIAN_POINT ( 'NONE',  ( 18.88192006459015815, -2.931848336738577920, 10.06696835938748613 ) ) ;
#21064 = CARTESIAN_POINT ( 'NONE',  ( -4.000000000000000000, 29.81534065533123723, 1.802053058880664471 ) ) ;
#21065 = CARTESIAN_POINT ( 'NONE',  ( 2.665366810462999947, 25.34956313825000151, 0.5220868594133000196 ) ) ;
#21066 = CARTESIAN_POINT ( 'NONE',  ( 2.185944241689015577, 13.92477108654476226, -5.721947785552420562 ) ) ;
#21067 = VECTOR ( 'NONE', #8863, 1000.000000000000000 ) ;
#21068 = B_SPLINE_CURVE_WITH_KNOTS ( 'NONE', 3,
 ( #16848, #12981, #4135, #20381, #6061 ),
 .UNSPECIFIED., .F., .F.,
 ( 4, 1, 4 ),
 ( 0.000000000000000000, 0.5000000000000000000, 1.000000000000000000 ),
 .UNSPECIFIED. ) ;
#21069 = LINE ( 'NONE', #17071, #18747 ) ;
#21070 = CARTESIAN_POINT ( 'NONE',  ( -24.27585716844903629, 12.49018833524722005, -3.366221553795681665 ) ) ;
#21071 = ADVANCED_FACE ( 'NONE', ( #8254 ), #7980, .F. ) ;
#21072 = CYLINDRICAL_SURFACE ( 'NONE', #23902, 2.649999999999999911 ) ;
#21073 = CARTESIAN_POINT ( 'NONE',  ( 14.51215565209456493, -7.098368344587701273, 5.661432951517745948 ) ) ;
#21074 = CARTESIAN_POINT ( 'NONE',  ( 18.65735837579211065, 4.963167965536912973, 9.221758217482731723 ) ) ;
#21075 = CARTESIAN_POINT ( 'NONE',  ( -4.544324455327999779, 13.49053734526000170, 5.132126114358000812 ) ) ;
#21076 = AXIS2_PLACEMENT_3D ( 'NONE', #7399, #23760, #18088 ) ;
#21077 = CARTESIAN_POINT ( 'NONE',  ( 61.60588651278290939, 74.97299614839606363, -1.000000000000000000 ) ) ;
#21078 = CARTESIAN_POINT ( 'NONE',  ( 12.52688711657000020, 7.716878364870000340, -11.63397459621999985 ) ) ;
#21079 = EDGE_LOOP ( 'NONE', ( #15264, #931, #7530, #12515, #15060 ) ) ;
#21080 = CARTESIAN_POINT ( 'NONE',  ( 7.500000000000000000, -10.00000000000000000, 0.000000000000000000 ) ) ;
#21081 = CARTESIAN_POINT ( 'NONE',  ( 11.53663804757020372, -12.55807338463293377, 3.248594360953877214 ) ) ;
#21082 = ORIENTED_EDGE ( 'NONE', *, *, #21974, .T. ) ;
#21083 = DIRECTION ( 'NONE',  ( 0.000000000000000000, -0.4362437346113740011, 0.8998285414523820025 ) ) ;
#21084 = DIRECTION ( 'NONE',  ( -0.5000000000000167644, 0.8660254037844290487, 0.000000000000000000 ) ) ;
#21085 = ADVANCED_FACE ( 'NONE', ( #2683 ), #4260, .T. ) ;
#21086 = CARTESIAN_POINT ( 'NONE',  ( -2.485727719834888827, 13.00711836349921846, 6.259936974863422599 ) ) ;
#21087 = CARTESIAN_POINT ( 'NONE',  ( 6.142597811584451506, 14.18464560812138409, -0.09518466390937729837 ) ) ;
#21088 = CARTESIAN_POINT ( 'NONE',  ( -6.803841411146002827, 15.25658587585999904, -2.419657731435000958 ) ) ;
#21089 = CARTESIAN_POINT ( 'NONE',  ( -6.707538334066213359, 15.26746356158001205, 2.299058024840869852 ) ) ;
#21090 = ORIENTED_EDGE ( 'NONE', *, *, #23079, .T. ) ;
#21091 = ORIENTED_EDGE ( 'NONE', *, *, #9180, .T. ) ;
#21092 = LINE ( 'NONE', #11420, #14579 ) ;
#21093 = CARTESIAN_POINT ( 'NONE',  ( 3.150855693196132457, 24.60222989789001957, 2.799640769041085164 ) ) ;
#21094 = CARTESIAN_POINT ( 'NONE',  ( 0.000000000000000000, 28.00000000000000000, 0.000000000000000000 ) ) ;
#21095 = VERTEX_POINT ( 'NONE', #13810 ) ;
#21096 = CARTESIAN_POINT ( 'NONE',  ( -23.61663544866999587, 6.459431347288000502, -7.956344550455000331 ) ) ;
#21097 = CARTESIAN_POINT ( 'NONE',  ( 1.719817536959529436, 12.95985172756701154, -1.059208683210195234 ) ) ;
#21098 = CARTESIAN_POINT ( 'NONE',  ( 6.145997960467107113, 14.15927157517049118, 0.1820614432005297212 ) ) ;
#21099 = CARTESIAN_POINT ( 'NONE',  ( 15.76307053266625857, -10.12283687570989521, 2.174611644706195612 ) ) ;
#21100 = CARTESIAN_POINT ( 'NONE',  ( -15.81542103158999701, -9.827833029818000554, -5.031439001898000640 ) ) ;
#21101 = ADVANCED_FACE ( 'NONE', ( #2431 ), #17325, .F. ) ;
#21102 = AXIS2_PLACEMENT_3D ( 'NONE', #2334, #504, #17343 ) ;
#21103 = CARTESIAN_POINT ( 'NONE',  ( -0.7612329563831000678, 28.57769546745999634, 2.100474675742999953 ) ) ;
#21104 = CARTESIAN_POINT ( 'NONE',  ( -19.68652699590384358, -7.391915032640794969, 7.432987506013617462 ) ) ;
#21105 = ADVANCED_FACE ( 'NONE', ( #11621 ), #7977, .T. ) ;
#21106 = CIRCLE ( 'NONE', #21496, 10.65000000000000036 ) ;
#21107 = CARTESIAN_POINT ( 'NONE',  ( 23.99062354302999722, 13.93375672974000068, -0.8660254037843999608 ) ) ;
#21108 = CARTESIAN_POINT ( 'NONE',  ( -0.5855206035033558853, 29.56888966826695508, 2.079019416249454633 ) ) ;
#21109 = ORIENTED_EDGE ( 'NONE', *, *, #8228, .F. ) ;
#21110 = CARTESIAN_POINT ( 'NONE',  ( 1.634731643160000081, 23.91997273684999925, 1.686691236754999990 ) ) ;
#21111 = CARTESIAN_POINT ( 'NONE',  ( -16.11254757976368168, -5.837216003886290139, 8.603859594677571110 ) ) ;
#21112 = ORIENTED_EDGE ( 'NONE', *, *, #19105, .T. ) ;
#21113 = CARTESIAN_POINT ( 'NONE',  ( 6.021392403978000907, 13.76381744684999830, -1.771980677399001669 ) ) ;
#21114 = ADVANCED_FACE ( 'NONE', ( #4229 ), #9677, .F. ) ;
#21115 = CARTESIAN_POINT ( 'NONE',  ( 0.6836813991273753555, 28.12756664670376594, 4.224074002598932509 ) ) ;
#21116 = EDGE_CURVE ( 'NONE', #4654, #12558, #17656, .T. ) ;
#21117 = LINE ( 'NONE', #2465, #11877 ) ;
#21118 = B_SPLINE_CURVE_WITH_KNOTS ( 'NONE', 3,
 ( #4844, #12230, #3152, #17920, #7008, #21676, #1445, #19618, #17805, #8841 ),
 .UNSPECIFIED., .F., .F.,
 ( 4, 2, 2, 2, 4 ),
 ( 0.000000000000000000, 0.2499999999999998890, 0.4999999999999997780, 0.7499999999999998890, 1.000000000000000000 ),
 .UNSPECIFIED. ) ;
#21119 =( BOUNDED_SURFACE ( )  B_SPLINE_SURFACE ( 3, 3, ( 
 ( #1758, #1878, #7432, #5398, #23910, #12783, #12437, #19821, #3235, #5971, #18589 ),
 ( #22678, #401, #4165, #13004, #1994, #22208, #13244, #20881, #9379, #14931, #17001 ),
 ( #18816, #11678, #18939, #9736, #9855, #22327, #11440, #2346, #11209, #518, #16749 ),
 ( #13353, #7798, #5743, #15056, #22449, #5861, #15285, #7919, #11326, #6086, #13480 ) ),
 .UNSPECIFIED., .F., .F., .T. ) 
 B_SPLINE_SURFACE_WITH_KNOTS ( ( 4, 4 ),
 ( 4, 1, 1, 1, 1, 1, 1, 1, 4 ),
 ( 0.000000000000000000, 1.000000000000000000 ),
 ( -0.005484827698312000517, 0.000000000000000000, 0.03886970175601000416, 0.08091373131045999367, 0.1291622851901999824, 0.1818598879200999940, 0.2344112070881000098, 0.2830789767138000013, 0.3223009594510999887 ),
 .UNSPECIFIED. ) 
 GEOMETRIC_REPRESENTATION_ITEM ( )  RATIONAL_B_SPLINE_SURFACE ( (
 ( 1.339323776348000150, 1.339323776348000150, 1.339323776348000150, 1.339323776348000150, 1.339323776348000150, 1.339323776348000150, 1.339323776348000150, 1.339323776348000150, 1.339323776348000150, 1.339323776348000150, 1.339323776348000150),
 ( 0.8868920745505000092, 0.8868920745505000092, 0.8868920745505000092, 0.8868920745505000092, 0.8868920745505000092, 0.8868920745505000092, 0.8868920745505000092, 0.8868920745505000092, 0.8868920745505000092, 0.8868920745505000092, 0.8868920745505000092),
 ( 0.8868920745505000092, 0.8868920745505000092, 0.8868920745505000092, 0.8868920745505000092, 0.8868920745505000092, 0.8868920745505000092, 0.8868920745505000092, 0.8868920745505000092, 0.8868920745505000092, 0.8868920745505000092, 0.8868920745505000092),
 ( 1.339323776348000150, 1.339323776348000150, 1.339323776348000150, 1.339323776348000150, 1.339323776348000150, 1.339323776348000150, 1.339323776348000150, 1.339323776348000150, 1.339323776348000150, 1.339323776348000150, 1.339323776348000150) ) ) 
 REPRESENTATION_ITEM ( '' )  SURFACE ( )  );
#21120 = CARTESIAN_POINT ( 'NONE',  ( 13.72218892130999990, -3.391610850449999770, -9.027048835217000189 ) ) ;
#21121 = ORIENTED_EDGE ( 'NONE', *, *, #5389, .F. ) ;
#21122 = CARTESIAN_POINT ( 'NONE',  ( 18.62128936713000371, -9.149140698829999252, 0.000000000000000000 ) ) ;
#21123 = LINE ( 'NONE', #886, #4939 ) ;
#21124 = LINE ( 'NONE', #2591, #10603 ) ;
#21125 = ORIENTED_EDGE ( 'NONE', *, *, #22878, .F. ) ;
#21126 = CARTESIAN_POINT ( 'NONE',  ( 0.000000000000000000, 19.00000000000000000, 0.000000000000000000 ) ) ;
#21127 = CARTESIAN_POINT ( 'NONE',  ( 21.09579166666667049, 9.212641304824277455, 1.205804979152653722 ) ) ;
#21128 = CARTESIAN_POINT ( 'NONE',  ( 24.20596017342987238, 1.317034122686029374, 10.54188528362805677 ) ) ;
#21129 = CARTESIAN_POINT ( 'NONE',  ( 18.93264468355999952, 0.000000000000000000, 0.000000000000000000 ) ) ;
#21130 = CARTESIAN_POINT ( 'NONE',  ( 18.32432198088978836, 7.518497202265214341, -7.212943697349772698 ) ) ;
#21131 = AXIS2_PLACEMENT_3D ( 'NONE', #14096, #19559, #17618 ) ;
#21132 = CARTESIAN_POINT ( 'NONE',  ( 1.768240990936880142, 24.49990546444021078, -1.767061324597003713 ) ) ;
#21133 = CARTESIAN_POINT ( 'NONE',  ( -14.40719418339326907, -8.953944931993278900, 9.491079701373102750 ) ) ;
#21134 = CARTESIAN_POINT ( 'NONE',  ( 23.57525185645999954, 10.70628383877999923, -3.581940172122999755 ) ) ;
#21135 = DIRECTION ( 'NONE',  ( 0.000000000000000000, 1.000000000000000000, 0.000000000000000000 ) ) ;
#21136 = CARTESIAN_POINT ( 'NONE',  ( -3.692138345368964014, 14.24529764263220066, -4.891414090216523292 ) ) ;
#21137 = CARTESIAN_POINT ( 'NONE',  ( -2.159773237450644423, 30.20518305836949224, 0.02532526672096173034 ) ) ;
#21138 = EDGE_LOOP ( 'NONE', ( #5110, #5576, #13977, #11030 ) ) ;
#21139 = CARTESIAN_POINT ( 'NONE',  ( 22.87199999999999989, 9.258222311379999070, 0.000000000000000000 ) ) ;
#21140 = CARTESIAN_POINT ( 'NONE',  ( 19.45402087125000179, 6.188800432692000975, -8.235960022457000207 ) ) ;
#21141 = CARTESIAN_POINT ( 'NONE',  ( 2.953635558952001361, 13.09662707700965889, -6.068300655576388536 ) ) ;
#21142 = CONICAL_SURFACE ( 'NONE', #6033, 4.699999872533999756, 0.7853981633972997312 ) ;
#21143 = CARTESIAN_POINT ( 'NONE',  ( 0.3272492347489454056, 27.65086340285666822, 2.499999999999998668 ) ) ;
#21144 = VECTOR ( 'NONE', #7565, 1000.000000000000114 ) ;
#21145 = CARTESIAN_POINT ( 'NONE',  ( -20.37651066538352040, 7.859203411085292856, -6.967962737658316641 ) ) ;
#21146 = DIRECTION ( 'NONE',  ( -1.000000000000000000, 0.000000000000000000, 0.000000000000000000 ) ) ;
#21147 = DIRECTION ( 'NONE',  ( 1.000000000000000000, 0.000000000000000000, 0.000000000000000000 ) ) ;
#21148 = ORIENTED_EDGE ( 'NONE', *, *, #3051, .F. ) ;
#21149 = CARTESIAN_POINT ( 'NONE',  ( -18.46587556182016243, 9.669871375868556385, -3.975206490073679877 ) ) ;
#21150 = CARTESIAN_POINT ( 'NONE',  ( 0.000000000000000000, 22.19999999999999574, 0.000000000000000000 ) ) ;
#21151 = AXIS2_PLACEMENT_3D ( 'NONE', #10245, #21510, #10614 ) ;
#21152 = CARTESIAN_POINT ( 'NONE',  ( -2.157506145421208554, 27.64352613552069116, 0.2337557657564511560 ) ) ;
#21153 = DIRECTION ( 'NONE',  ( 0.000000000000000000, 0.000000000000000000, 1.000000000000000000 ) ) ;
#21154 = AXIS2_PLACEMENT_3D ( 'NONE', #11507, #18881, #15479 ) ;
#21155 = CARTESIAN_POINT ( 'NONE',  ( 11.47028936713000036, -8.379193606113998882, -3.189305674207999708 ) ) ;
#21156 = EDGE_LOOP ( 'NONE', ( #12318, #22550, #9431, #3968, #9781 ) ) ;
#21157 = CARTESIAN_POINT ( 'NONE',  ( 0.000000000000000000, 15.09999999999999964, 0.000000000000000000 ) ) ;
#21158 = AXIS2_PLACEMENT_3D ( 'NONE', #20580, #7497, #110 ) ;
#21159 = CARTESIAN_POINT ( 'NONE',  ( 17.06568924931000097, -1.008082813539000089, 10.70191082552000061 ) ) ;
#21160 = CARTESIAN_POINT ( 'NONE',  ( -21.00779098860000005, -8.370598903416999192, -7.355548942906000143 ) ) ;
#21161 = CARTESIAN_POINT ( 'NONE',  ( -13.46246977166000036, 9.006734844048001065, -4.712226836624999748 ) ) ;
#21162 = CARTESIAN_POINT ( 'NONE',  ( 22.00279166666665631, -9.235916712427657771, -1.208851722883304225 ) ) ;
#21163 = CARTESIAN_POINT ( 'NONE',  ( 17.63056994525999954, 1.419371566880999858, 10.23411406235000065 ) ) ;
#21164 = CARTESIAN_POINT ( 'NONE',  ( -0.4496761300970291142, 28.77800341527711936, 2.126187163699609251 ) ) ;
#21165 = B_SPLINE_CURVE_WITH_KNOTS ( 'NONE', 3,
 ( #1351, #18066, #7380, #18409, #6917, #3531, #3418, #21703, #9205, #5457, #16584, #18194, #10913, #3638, #1700, #3296, #3992, #10801, #21813, #1473, #16238, #23629, #14652, #17945, #22048, #8978, #16104, #9090, #8741, #19880, #14311, #7035, #5340, #19998, #23739, #14762, #23851, #12840, #22160, #14421, #16350, #16461 ),
 .UNSPECIFIED., .F., .F.,
 ( 4, 2, 1, 2, 2, 2, 1, 2, 2, 2, 2, 2, 2, 2, 2, 1, 2, 2, 2, 1, 2, 2, 4 ),
 ( 0.000000000000000000, 0.06250000000000038858, 0.09375000000000058287, 0.1093750000000006800, 0.1250000000000007772, 0.1875000000000011102, 0.2187500000000012768, 0.2343750000000013045, 0.2500000000000013323, 0.3125000000000011657, 0.3750000000000009992, 0.5000000000000006661, 0.5625000000000004441, 0.6250000000000003331, 0.6875000000000001110, 0.7187500000000000000, 0.7343749999999998890, 0.7499999999999997780, 0.8124999999999997780, 0.8437499999999997780, 0.8593749999999996669, 0.8749999999999995559, 1.000000000000000000 ),
 .UNSPECIFIED. ) ;
#21166 = CARTESIAN_POINT ( 'NONE',  ( 0.6543697108982093891, 26.86753006952333678, 2.434931691670787490 ) ) ;
#21167 = CARTESIAN_POINT ( 'NONE',  ( 23.24015326692000016, 4.650820575430000048, 8.573381078705001102 ) ) ;
#21168 = CARTESIAN_POINT ( 'NONE',  ( 6.243179582884000212, 13.63342035941999875, -1.952365010387999922 ) ) ;
#21169 = ORIENTED_EDGE ( 'NONE', *, *, #4994, .T. ) ;
#21170 = CARTESIAN_POINT ( 'NONE',  ( 1.314425600296815544, 13.77569882054628359, 5.982788395604068832 ) ) ;
#21171 = CARTESIAN_POINT ( 'NONE',  ( 2.644546391786999795, 26.77206776951999956, -0.3657850755363000195 ) ) ;
#21172 = CARTESIAN_POINT ( 'NONE',  ( 4.739989412068003283, 12.46385783664001323, 0.6598078427890002873 ) ) ;
#21173 = CARTESIAN_POINT ( 'NONE',  ( 2.052791027186419814, 28.96347044016121686, 0.6716916050526000603 ) ) ;
#21174 = CARTESIAN_POINT ( 'NONE',  ( -24.08729801477999999, 11.11025767225000038, 1.070257339459000034 ) ) ;
#21175 = LINE ( 'NONE', #20936, #6131 ) ;
#21176 = EDGE_LOOP ( 'NONE', ( #17740, #10082, #493, #17129, #19964 ) ) ;
#21177 = CARTESIAN_POINT ( 'NONE',  ( 15.06887270046331651, -8.822272326497644812, -2.370789473217528087 ) ) ;
#21178 = AXIS2_PLACEMENT_3D ( 'NONE', #11832, #19212, #5891 ) ;
#21179 = CARTESIAN_POINT ( 'NONE',  ( 0.4925334044481964879, 26.25981921813487219, 2.102983069868059385 ) ) ;
#21180 = CARTESIAN_POINT ( 'NONE',  ( -1.497298415485000200, 13.90645643049002089, 5.974715374002997237 ) ) ;
#21181 = CARTESIAN_POINT ( 'NONE',  ( -1.779764907139927077, 26.49975665830813298, 1.755621799651315262 ) ) ;
#21182 = FACE_OUTER_BOUND ( 'NONE', #7174, .T. ) ;
#21183 = EDGE_CURVE ( 'NONE', #22057, #13042, #5657, .T. ) ;
#21184 = CARTESIAN_POINT ( 'NONE',  ( 1.259047450927247569, 27.16753006952333038, -2.184465970885645536 ) ) ;
#21185 = CARTESIAN_POINT ( 'NONE',  ( -6.201796767088660900, 15.80323617239661260, -1.134441279322979668 ) ) ;
#21186 = AXIS2_PLACEMENT_3D ( 'NONE', #11822, #2614, #11466 ) ;
#21187 = CARTESIAN_POINT ( 'NONE',  ( 16.76700125730999957, -9.205641116351999997, -0.3944625347444000174 ) ) ;
#21188 = CARTESIAN_POINT ( 'NONE',  ( 24.37173283531060264, 3.055078579629053159, 12.50000000000000533 ) ) ;
#21189 = B_SPLINE_CURVE_WITH_KNOTS ( 'NONE', 3,
 ( #13400, #5895, #11718, #9774, #15209 ),
 .UNSPECIFIED., .F., .F.,
 ( 4, 1, 4 ),
 ( 0.000000000000000000, 0.5000000000000000000, 1.000000000000000000 ),
 .UNSPECIFIED. ) ;
#21190 = VERTEX_POINT ( 'NONE', #4466 ) ;
#21191 = CARTESIAN_POINT ( 'NONE',  ( -22.83407172560354326, 9.257125376469652167, 1.211339697711120156 ) ) ;
#21192 = CARTESIAN_POINT ( 'NONE',  ( 0.9860083823784999701, 30.79379877136000232, -2.124103741218000163 ) ) ;
#21193 = CARTESIAN_POINT ( 'NONE',  ( -15.20062077250666377, 1.186002250417414805, 9.061359600907872291 ) ) ;
#21194 = CARTESIAN_POINT ( 'NONE',  ( 1.859456552709266575, 13.85899723262824423, -5.839145259044595804 ) ) ;
#21195 = CARTESIAN_POINT ( 'NONE',  ( 20.89481827668999969, 1.510888802920000051, 11.11378095030000068 ) ) ;
#21196 = DIRECTION ( 'NONE',  ( 1.000000000000000000, 0.000000000000000000, 0.000000000000000000 ) ) ;
#21197 = EDGE_CURVE ( 'NONE', #4978, #21807, #3508, .T. ) ;
#21198 = CARTESIAN_POINT ( 'NONE',  ( 11.36701043058742044, 2.759410678195907352, 12.49996441860552743 ) ) ;
#21199 = CARTESIAN_POINT ( 'NONE',  ( 16.56656853291420006, 10.34692677961490226, 1.231521008520755966 ) ) ;
#21200 = DIRECTION ( 'NONE',  ( 0.000000000000000000, 1.000000000000000000, 0.000000000000000000 ) ) ;
#21201 = CARTESIAN_POINT ( 'NONE',  ( -21.20949577250664575, 8.052478750070527269, -4.641013231564889985 ) ) ;
#21202 = CARTESIAN_POINT ( 'NONE',  ( 24.36881528991174406, -12.37037615450637240, -3.573879991655171562 ) ) ;
#21203 = ORIENTED_EDGE ( 'NONE', *, *, #8544, .T. ) ;
#21204 = CARTESIAN_POINT ( 'NONE',  ( -24.50000000000001066, -9.922076442417122166, -2.874310295333110332 ) ) ;
#21205 = DIRECTION ( 'NONE',  ( -1.000000000000000000, 0.000000000000000000, 0.000000000000000000 ) ) ;
#21206 = AXIS2_PLACEMENT_3D ( 'NONE', #600, #6054, #22644 ) ;
#21207 = ORIENTED_EDGE ( 'NONE', *, *, #668, .F. ) ;
#21208 = B_SPLINE_SURFACE_WITH_KNOTS ( 'NONE', 3, 3, ( 
 ( #14407, #17818, #3404, #18393, #12828, #16447, #9074, #16685, #16335, #1686, #207, #23835, #9311, #5445, #95, #13173, #18512, #5326, #7131, #9429, #3518, #10899, #18631, #12933, #7246, #7600, #14635, #14979, #22036, #23961, #5555, #20220, #20331, #3626, #22252 ),
 ( #1804, #3862, #3737, #21913, #8965, #11253, #23725, #9192, #11009, #22375, #16569, #11127, #20562, #7365, #16800, #1924, #7480, #14862, #12714, #14521, #5668, #5790, #14750, #13054, #20449, #2039, #3977, #22146, #18180, #1581, #20109, #18286, #2270, #13285, #18742 ),
 ( #6140, #16922, #19224, #22490, #13404, #20805, #559, #20684, #324, #4093, #4214, #2153, #7966, #11489, #13765, #8211, #22727, #2388, #18865, #13529, #11608, #15337, #812, #8094, #22847, #22966, #9664, #20926, #15462, #7729, #13644, #5900, #17417, #2509, #4331 ),
 ( #6260, #15213, #17044, #15095, #21039, #6381, #442, #11723, #7845, #22610, #6019, #17287, #9899, #21167, #11370, #11845, #4454, #9779, #2637, #688, #10032, #18979, #19097, #17164, #15578, #9543, #19723, #17658, #17785, #2885, #16059, #6744, #19600, #4824, #8695 ) ),
 .UNSPECIFIED., .F., .F., .F.,
 ( 4, 4 ),
 ( 4, 1, 1, 1, 1, 1, 1, 1, 1, 1, 1, 1, 1, 1, 1, 1, 1, 1, 1, 1, 1, 1, 1, 1, 1, 1, 1, 1, 1, 1, 1, 1, 4 ),
 ( -0.08331297109794000288, 1.083312971098000066 ),
 ( 0.1767973369902999803, 0.2030268336058000112, 0.2292563302213000143, 0.2554858268368000451, 0.2817153234522999927, 0.3079448200677999958, 0.3341743166833000545, 0.3604038132988000021, 0.3866333099143000052, 0.4128628065298000083, 0.4390923031453000114, 0.4653217997607999590, 0.4915512963763000176, 0.5177807929918000207, 0.5440102896073000238, 0.5702397862229000580, 0.5964692828384000611, 0.6226987794539000642, 0.6489282760694000673, 0.6751577726849000705, 0.7013872693004000736, 0.7276167659159000767, 0.7538462625314000798, 0.7800757591469000829, 0.8063052557624000860, 0.8325347523779000891, 0.8587642489933999812, 0.8849937456089000953, 0.9112232422244000984, 0.9374527388398999905, 0.9636822354555000247, 0.9899117320710000278, 1.016141228685999875 ),
 .UNSPECIFIED. ) ;
#21209 = CARTESIAN_POINT ( 'NONE',  ( 2.614613892538000250, 26.07965299175999974, -0.4120747533924999928 ) ) ;
#21210 = CARTESIAN_POINT ( 'NONE',  ( -1.681586879633373721, 24.51484633230852950, -1.409227352623252827 ) ) ;
#21211 = CARTESIAN_POINT ( 'NONE',  ( -2.924596640938022851, 13.09248804016575285, 6.076189607320904074 ) ) ;
#21212 = B_SPLINE_CURVE_WITH_KNOTS ( 'NONE', 3,
 ( #4742, #4617, #8367, #19390, #17698, #15859, #14055, #15736, #1095, #21448 ),
 .UNSPECIFIED., .F., .F.,
 ( 4, 2, 2, 2, 4 ),
 ( 0.000000000000000000, 0.1249999999999998890, 0.2499999999999997780, 0.4999999999999998890, 1.000000000000000000 ),
 .UNSPECIFIED. ) ;
#21213 = CARTESIAN_POINT ( 'NONE',  ( 6.154459514182900826, 14.10386533427145395, -0.3250634448250298014 ) ) ;
#21214 = CARTESIAN_POINT ( 'NONE',  ( -6.460131137950000380, 15.34438815028998704, -0.9341689219261994914 ) ) ;
#21215 = AXIS2_PLACEMENT_3D ( 'NONE', #9286, #14171, #5101 ) ;
#21216 = VECTOR ( 'NONE', #815, 1000.000000000000000 ) ;
#21217 = ADVANCED_FACE ( 'NONE', ( #1195 ), #6440, .T. ) ;
#21218 = CARTESIAN_POINT ( 'NONE',  ( -6.249999999916000526, 15.09564573669999987, 3.212813967733000098 ) ) ;
#21219 = ORIENTED_EDGE ( 'NONE', *, *, #15602, .T. ) ;
#21220 = EDGE_LOOP ( 'NONE', ( #4024, #20272, #6182, #14356, #17640, #22656 ) ) ;
#21221 = DIRECTION ( 'NONE',  ( 0.000000000000000000, 0.000000000000000000, -1.000000000000000000 ) ) ;
#21222 = DIRECTION ( 'NONE',  ( 0.7071067811865465735, 0.7071067811865465735, 5.135208691342337292E-08 ) ) ;
#21223 = DIRECTION ( 'NONE',  ( 0.000000000000000000, 1.000000000000000000, 0.000000000000000000 ) ) ;
#21224 = EDGE_LOOP ( 'NONE', ( #9588, #15420, #12584, #16748 ) ) ;
#21225 = CARTESIAN_POINT ( 'NONE',  ( -20.63087924974999865, -6.603491279182000184, 7.028696436783999246 ) ) ;
#21226 = CARTESIAN_POINT ( 'NONE',  ( 1.800000000000000044, 13.00000000000000000, -1.081665382638999917 ) ) ;
#21227 = CARTESIAN_POINT ( 'NONE',  ( -1.181632374603358793, 28.05137445130588603, -3.936586548166617572 ) ) ;
#21228 = CARTESIAN_POINT ( 'NONE',  ( 14.99956892033451972, 9.898833753622279019, 2.972387950973069959 ) ) ;
#21229 = CIRCLE ( 'NONE', #20842, 2.000000000000000000 ) ;
#21230 = CARTESIAN_POINT ( 'NONE',  ( -19.72979285727999965, -9.249309651556000489, 5.317383783821999721 ) ) ;
#21231 = CARTESIAN_POINT ( 'NONE',  ( 0.2336534512014000198, 29.00931759149999678, -2.344603603009000281 ) ) ;
#21232 = ADVANCED_FACE ( 'NONE', ( #23343 ), #10647, .T. ) ;
#21233 = CARTESIAN_POINT ( 'NONE',  ( -20.12402413361354903, 7.018225891280687634, 7.806669810472256721 ) ) ;
#21234 = CARTESIAN_POINT ( 'NONE',  ( 1.371414133342000685, 11.63072304285000236, -4.560271503704002249 ) ) ;
#21235 = CARTESIAN_POINT ( 'NONE',  ( -15.06773579844999844, 6.079600582824999933, -9.557752359651999541 ) ) ;
#21236 = CARTESIAN_POINT ( 'NONE',  ( -1.090704560478623186, 29.53635738603347249, 1.864235603192405222 ) ) ;
#21237 = VERTEX_POINT ( 'NONE', #1067 ) ;
#21238 = CARTESIAN_POINT ( 'NONE',  ( -2.146635823351999761, 25.21280799190000010, 0.4123919462612000153 ) ) ;
#21239 = CARTESIAN_POINT ( 'NONE',  ( -16.05466923206691021, -7.433158090429714093, 7.276088876722277554 ) ) ;
#21240 = VERTEX_POINT ( 'NONE', #14031 ) ;
#21241 = CARTESIAN_POINT ( 'NONE',  ( 2.053005267516999902E-14, 28.63049582772000079, 2.160000000000000142 ) ) ;
#21242 = CARTESIAN_POINT ( 'NONE',  ( 5.808047881160999459, 14.58015161914997648, -1.975228513291002574 ) ) ;
#21243 = CLOSED_SHELL ( 'NONE', ( #2498, #22582, #6699, #18016, #13663, #20712, #13038, #9838, #23755, #16651, #20511, #5420, #12373, #8931, #23282, #6720, #11744, #21665, #6104, #8528, #12181, #22780, #21852, #5269, #2918, #3471, #15695, #8243, #19196, #16874 ) ) ;
#21244 = DIRECTION ( 'NONE',  ( 0.000000000000000000, 1.000000000000000000, 0.000000000000000000 ) ) ;
#21245 = AXIS2_PLACEMENT_3D ( 'NONE', #8610, #15972, #17937 ) ;
#21246 = DIRECTION ( 'NONE',  ( 0.000000000000000000, 1.000000000000000000, 0.000000000000000000 ) ) ;
#21247 = ADVANCED_FACE ( 'NONE', ( #7002, #1318 ), #21422, .F. ) ;
#21248 = CARTESIAN_POINT ( 'NONE',  ( 16.24500142131000047, 8.402176888622001627, 4.865949138796000106 ) ) ;
#21249 = ADVANCED_FACE ( 'NONE', ( #2775 ), #14153, .F. ) ;
#21250 = VERTEX_POINT ( 'NONE', #4961 ) ;
#21251 = CARTESIAN_POINT ( 'NONE',  ( -8.721209826254002095, 12.89567489919000032, -6.006002783705000070 ) ) ;
#21252 = DIRECTION ( 'NONE',  ( -1.000000000000000000, 0.000000000000000000, 0.000000000000000000 ) ) ;
#21253 = CARTESIAN_POINT ( 'NONE',  ( 0.000000000000000000, 22.00131761696259503, 0.000000000000000000 ) ) ;
#21254 = CIRCLE ( 'NONE', #18191, 2.399999999999999911 ) ;
#21255 = ORIENTED_EDGE ( 'NONE', *, *, #2867, .T. ) ;
#21256 = CARTESIAN_POINT ( 'NONE',  ( -1.042632460611140788, 24.73976796275902146, 1.891962004173780576 ) ) ;
#21257 = CARTESIAN_POINT ( 'NONE',  ( 0.000000000000000000, 22.00000000000000000, 0.000000000000000000 ) ) ;
#21258 = CARTESIAN_POINT ( 'NONE',  ( 4.815594511070003136, 12.64391016021000702, -0.02336859300116998425 ) ) ;
#21259 = CARTESIAN_POINT ( 'NONE',  ( -13.99999999999999645, -7.071987877914798659, 7.398104326063183578 ) ) ;
#21261 = CARTESIAN_POINT ( 'NONE',  ( 16.27419025256129004, -0.09153522013711405669, -10.36548162492280412 ) ) ;
#21260 = AXIS2_PLACEMENT_3D ( 'NONE', #13925, #4980, #2916 ) ;
#21262 = DIRECTION ( 'NONE',  ( 1.000000000000000000, -0.000000000000000000, -0.000000000000000000 ) ) ;
#21263 = DIRECTION ( 'NONE',  ( 0.000000000000000000, -1.000000000000000000, 0.000000000000000000 ) ) ;
#21265 = EDGE_CURVE ( 'NONE', #1933, #2511, #8774, .T. ) ;
#21264 = CARTESIAN_POINT ( 'NONE',  ( 19.35367170822999938, -8.078004626089001050, -7.719962156281999555 ) ) ;
#21266 = EDGE_CURVE ( 'NONE', #18791, #20510, #21922, .T. ) ;
#21267 = CARTESIAN_POINT ( 'NONE',  ( -0.9744765624120645953, 26.41693820796410819, 4.056187847889995979 ) ) ;
#21268 = B_SPLINE_CURVE_WITH_KNOTS ( 'NONE', 3,
 ( #19076, #2132, #9521, #7708, #15557, #6724, #13743, #10371, #21143, #23427, #2744, #17635, #1034, #4802, #17513, #4557, #907, #6361 ),
 .UNSPECIFIED., .F., .F.,
 ( 4, 2, 2, 2, 2, 2, 2, 2, 4 ),
 ( 0.000000000000000000, 0.1250000000000000000, 0.2500000000000000000, 0.3750000000000000000, 0.5000000000000000000, 0.6250000000000000000, 0.7500000000000000000, 0.8750000000000000000, 1.000000000000000000 ),
 .UNSPECIFIED. ) ;
#21269 = DIRECTION ( 'NONE',  ( 0.000000000000000000, 1.000000000000000000, 0.000000000000000000 ) ) ;
#21270 = DIRECTION ( 'NONE',  ( 0.000000000000000000, 1.000000000000000000, 0.000000000000000000 ) ) ;
#21271 = CARTESIAN_POINT ( 'NONE',  ( -1.180412381323944881, 30.07751909137916613, -1.808792577990875783 ) ) ;
#21272 = ORIENTED_EDGE ( 'NONE', *, *, #15458, .T. ) ;
#21273 = CARTESIAN_POINT ( 'NONE',  ( 18.48776620345000055, -4.367899469603999663, 9.299952195460999604 ) ) ;
#21274 = CARTESIAN_POINT ( 'NONE',  ( 23.98778900788900970, 10.71396164900311021, 0.03587804490455098749 ) ) ;
#21275 = CARTESIAN_POINT ( 'NONE',  ( -2.136729350344353850, 23.63672935034427880, -0.2192973291338879971 ) ) ;
#21276 = VECTOR ( 'NONE', #17029, 1000.000000000000000 ) ;
#21277 = CARTESIAN_POINT ( 'NONE',  ( -20.45683979044500944, 5.645737104002305884, -8.860185778984789096 ) ) ;
#21278 = DIRECTION ( 'NONE',  ( -1.000000000000000000, 0.000000000000000000, 0.000000000000000000 ) ) ;
#21279 = CARTESIAN_POINT ( 'NONE',  ( 3.897341104911002940, 12.15007725568001362, -3.081013383565999852 ) ) ;
#21280 = VERTEX_POINT ( 'NONE', #17800 ) ;
#21281 = CARTESIAN_POINT ( 'NONE',  ( -16.12133163457191287, 1.276676612278212497, 10.31581741333146240 ) ) ;
#21282 = CARTESIAN_POINT ( 'NONE',  ( -3.999999999999999112, 29.79977277844470862, -1.897803675662255163 ) ) ;
#21283 = AXIS2_PLACEMENT_3D ( 'NONE', #16797, #6017, #18977 ) ;
#21284 = CARTESIAN_POINT ( 'NONE',  ( 0.3677801680678270402, 26.60799041457681113, -2.168894944354226695 ) ) ;
#21285 =( LENGTH_UNIT ( ) NAMED_UNIT ( * ) SI_UNIT ( .MILLI., .METRE. ) );
#21286 = DIRECTION ( 'NONE',  ( -1.000000000000000000, 0.000000000000000000, 0.000000000000000000 ) ) ;
#21287 = EDGE_LOOP ( 'NONE', ( #5911, #10943, #14097, #12647 ) ) ;
#21288 = DIRECTION ( 'NONE',  ( 0.000000000000000000, 1.000000000000000000, 0.000000000000000000 ) ) ;
#21289 = CARTESIAN_POINT ( 'NONE',  ( -12.02109039332999885, 12.23011958036999935, -9.372058967585999767 ) ) ;
#21290 = CARTESIAN_POINT ( 'NONE',  ( -20.36544424872999670, 10.91338584732999983, -2.163915618822000120 ) ) ;
#21291 = CARTESIAN_POINT ( 'NONE',  ( -16.10150461667999977, -7.663156287736000216, -6.860248635285000063 ) ) ;
#21292 = CARTESIAN_POINT ( 'NONE',  ( -6.307433260514002882, 15.63766309337001204, 1.260389944764000125 ) ) ;
#21293 = CARTESIAN_POINT ( 'NONE',  ( 13.22952827859000102, 3.056853952720000045, -9.159678806024000863 ) ) ;
#21294 = CARTESIAN_POINT ( 'NONE',  ( -2.197883833863924163, 28.59249535265084674, -0.2145651371980360489 ) ) ;
#21295 = CARTESIAN_POINT ( 'NONE',  ( 2.404489386789158356, 26.49040384242090695, -3.230569558791225315 ) ) ;
#21296 = DIRECTION ( 'NONE',  ( -1.000000000000000000, 0.000000000000000000, 0.000000000000000000 ) ) ;
#21297 = EDGE_LOOP ( 'NONE', ( #21452, #13456, #21029, #18381, #15200, #12441 ) ) ;
#21298 = CARTESIAN_POINT ( 'NONE',  ( -2.168773205512959823, 13.92118792069584998, 5.728215446730930971 ) ) ;
#21299 = CARTESIAN_POINT ( 'NONE',  ( -0.2222064166829000043, 26.75619850838000247, -2.256099604565999783 ) ) ;
#21300 = DIRECTION ( 'NONE',  ( -0.7071067811823850136, -0.7071067811898851252, -1.080116769369976149E-06 ) ) ;
#21301 = CARTESIAN_POINT ( 'NONE',  ( -21.58102982807999837, -8.846676569589000394, 6.693734360802999994 ) ) ;
#21302 = CARTESIAN_POINT ( 'NONE',  ( -6.000000000000000000, 28.00000000000000000, 1.229194263906999929 ) ) ;
#21303 = VERTEX_POINT ( 'NONE', #19737 ) ;
#21304 = DIRECTION ( 'NONE',  ( 0.000000000000000000, 0.000000000000000000, -1.000000000000000000 ) ) ;
#21305 = DIRECTION ( 'NONE',  ( -1.000000000000000000, 0.000000000000000000, 0.000000000000000000 ) ) ;
#21306 = CARTESIAN_POINT ( 'NONE',  ( -0.7783053373570000266, 28.00000000000000000, 6.000000000000000000 ) ) ;
#21307 = CARTESIAN_POINT ( 'NONE',  ( -0.4015214144528502782, 6.789688267195424842, 1.702981870680819521 ) ) ;
#21308 = CARTESIAN_POINT ( 'NONE',  ( -24.00016455340000121, 1.715543117993999783E-14, -9.787173237795000702 ) ) ;
#21309 = FACE_OUTER_BOUND ( 'NONE', #7913, .T. ) ;
#21310 = CARTESIAN_POINT ( 'NONE',  ( -13.64582336266999896, -8.030615239332000499, -7.932400521014000283 ) ) ;
#21311 = CARTESIAN_POINT ( 'NONE',  ( 12.48918875731000000, 5.414613097170000167, 7.315858880121999697 ) ) ;
#21312 = CARTESIAN_POINT ( 'NONE',  ( 18.93546403748226936, 2.261952095453904299, 10.18648252659528453 ) ) ;
#21313 = ORIENTED_EDGE ( 'NONE', *, *, #11200, .F. ) ;
#21314 = CARTESIAN_POINT ( 'NONE',  ( -0.3272492347489393549, 28.61666666666667069, -2.499999999999999556 ) ) ;
#21315 = CARTESIAN_POINT ( 'NONE',  ( -2.375513208737999982, 29.50945927196000085, -0.8786735848391999948 ) ) ;
#21316 = CARTESIAN_POINT ( 'NONE',  ( -15.01166243917333176, -4.561147897106140547, 7.913407070503003737 ) ) ;
#21317 = CARTESIAN_POINT ( 'NONE',  ( 3.087353659563723873, 14.15392277165757662, -5.289980554907421251 ) ) ;
#21318 = CIRCLE ( 'NONE', #25, 1.500000000000000222 ) ;
#21319 = CARTESIAN_POINT ( 'NONE',  ( -12.75000000000000000, 0.000000000000000000, 0.000000000000000000 ) ) ;
#21320 = CYLINDRICAL_SURFACE ( 'NONE', #2686, 0.09999999999999939493 ) ;
#21321 = CARTESIAN_POINT ( 'NONE',  ( 0.5025988904459999240, 29.55075530783999938, -2.699273784843000179 ) ) ;
#21322 = DIRECTION ( 'NONE',  ( 0.000000000000000000, -1.000000000000000000, 0.000000000000000000 ) ) ;
#21323 = CARTESIAN_POINT ( 'NONE',  ( 15.53511221042325907, -9.890698584888076184, 3.204571028146030010 ) ) ;
#21324 = LINE ( 'NONE', #17319, #1764 ) ;
#21325 = FACE_OUTER_BOUND ( 'NONE', #3835, .T. ) ;
#21326 = EDGE_CURVE ( 'NONE', #14748, #9720, #7589, .T. ) ;
#21327 = CARTESIAN_POINT ( 'NONE',  ( 0.000000000000000000, 7.000000000000000000, 0.000000000000000000 ) ) ;
#21328 = ORIENTED_EDGE ( 'NONE', *, *, #17236, .F. ) ;
#21329 = LINE ( 'NONE', #23250, #23571 ) ;
#21330 = CARTESIAN_POINT ( 'NONE',  ( 11.22285964979965023, -11.82554192023893158, 4.517540867111200953 ) ) ;
#21331 = ORIENTED_EDGE ( 'NONE', *, *, #15253, .T. ) ;
#21332 = CARTESIAN_POINT ( 'NONE',  ( -2.208934844301000400, 25.40431520043999924, -0.8113325475626999017 ) ) ;
#21333 = CARTESIAN_POINT ( 'NONE',  ( 2.170273952127825812, 24.22245577580034848, -0.3150010920229354139 ) ) ;
#21334 = CARTESIAN_POINT ( 'NONE',  ( 2.190908539898643426, 12.96599634601801831, 6.341814094140324265 ) ) ;
#21335 = CARTESIAN_POINT ( 'NONE',  ( 6.156454711165042504, 14.09190061863668575, -0.3541682061968411399 ) ) ;
#21336 = DIRECTION ( 'NONE',  ( 0.000000000000000000, 0.000000000000000000, -1.000000000000000000 ) ) ;
#21337 = CARTESIAN_POINT ( 'NONE',  ( 0.1690226414553999690, 27.16669433610000084, -2.866097959738999723 ) ) ;
#21338 = ADVANCED_FACE ( 'NONE', ( #3148 ), #16071, .T. ) ;
#21339 = ORIENTED_EDGE ( 'NONE', *, *, #13472, .T. ) ;
#21340 = CARTESIAN_POINT ( 'NONE',  ( -12.35782623356324095, 9.652455568630072591, -11.96866129963372849 ) ) ;
#21341 = DIRECTION ( 'NONE',  ( 0.000000000000000000, -1.000000000000000000, 0.000000000000000000 ) ) ;
#21342 = CARTESIAN_POINT ( 'NONE',  ( 0.000000000000000000, 16.89999999999999858, -4.749999999999985789 ) ) ;
#21343 = VERTEX_POINT ( 'NONE', #21783 ) ;
#21344 = CARTESIAN_POINT ( 'NONE',  ( -20.53203420772999976, -9.474484991426001201, -3.680778544930999985 ) ) ;
#21345 = CARTESIAN_POINT ( 'NONE',  ( 1.709407021842912489, 12.94283542261882047, -1.056280950884417091 ) ) ;
#21346 = CARTESIAN_POINT ( 'NONE',  ( 20.22658333333333047, -8.951184447692499546, -2.405433643222833151 ) ) ;
#21347 = CARTESIAN_POINT ( 'NONE',  ( 15.24105989044193166, 4.435666536080931976, 9.339999123369469913 ) ) ;
#21348 = CARTESIAN_POINT ( 'NONE',  ( -17.26072755184999963, 1.977436118132999798, -10.90262414946000114 ) ) ;
#21349 = CARTESIAN_POINT ( 'NONE',  ( -2.020778351004999696, 29.15319163284999959, -1.211699210884999989 ) ) ;
#21350 = CARTESIAN_POINT ( 'NONE',  ( -23.01857833252245911, 8.092376861233656626, 4.663496906030524691 ) ) ;
#21351 = CARTESIAN_POINT ( 'NONE',  ( -4.097103695893997255, 12.37558244084000059, -2.395384390973998467 ) ) ;
#21352 = DIRECTION ( 'NONE',  ( 1.000000000000000000, 0.000000000000000000, 0.000000000000000000 ) ) ;
#21353 = EDGE_CURVE ( 'NONE', #17213, #17895, #23471, .T. ) ;
#21354 = CARTESIAN_POINT ( 'NONE',  ( -1.423014976520625474, 29.51237747527418520, 1.625193323046951743 ) ) ;
#21355 = VERTEX_POINT ( 'NONE', #12103 ) ;
#21356 = PLANE ( 'NONE',  #12269 ) ;
#21357 = CARTESIAN_POINT ( 'NONE',  ( -17.35693205524438909, -5.675076331185680445, -8.750869078049179350 ) ) ;
#21358 = ORIENTED_EDGE ( 'NONE', *, *, #20251, .F. ) ;
#21359 = CARTESIAN_POINT ( 'NONE',  ( -23.75392853996000042, 6.467096933425000138, -12.35553624208999857 ) ) ;
#21360 = CARTESIAN_POINT ( 'NONE',  ( 6.131903631775997177, 14.49480975922001491, 0.05943612597242994150 ) ) ;
#21361 = CARTESIAN_POINT ( 'NONE',  ( 0.000000000000000000, 28.30000000000000071, 4.618802153517000519 ) ) ;
#21362 = AXIS2_PLACEMENT_3D ( 'NONE', #9450, #11393, #11745 ) ;
#21363 = CARTESIAN_POINT ( 'NONE',  ( 17.58116666666665395, 7.971120433115317816, 4.594121230069161399 ) ) ;
#21364 = EDGE_CURVE ( 'NONE', #13406, #11582, #15311, .T. ) ;
#21365 = CARTESIAN_POINT ( 'NONE',  ( 15.06487658531000129, -2.993859790429000078, 9.737735315623000432 ) ) ;
#21366 = EDGE_LOOP ( 'NONE', ( #12051, #15618 ) ) ;
#21367 = DIRECTION ( 'NONE',  ( 0.000000000000000000, 0.000000000000000000, -1.000000000000000000 ) ) ;
#21368 = DIRECTION ( 'NONE',  ( -0.000000000000000000, -1.000000000000000000, -0.000000000000000000 ) ) ;
#21369 = ORIENTED_EDGE ( 'NONE', *, *, #22155, .T. ) ;
#21370 = CARTESIAN_POINT ( 'NONE',  ( 11.12576011241313090, 11.44859199039787789, 5.170472096583769606 ) ) ;
#21371 = DIRECTION ( 'NONE',  ( 0.000000000000000000, -1.000000000000000000, 0.000000000000000000 ) ) ;
#21372 = VECTOR ( 'NONE', #20270, 1000.000000000000000 ) ;
#21373 = CARTESIAN_POINT ( 'NONE',  ( -4.820914651057999656, 13.20110358117000082, -5.836454220812999694 ) ) ;
#21374 = CARTESIAN_POINT ( 'NONE',  ( 16.28472136693522998, 0.2845602576508600157, -10.36427326206977462 ) ) ;
#21375 = ADVANCED_FACE ( 'NONE', ( #23598 ), #240, .T. ) ;
#21376 = CARTESIAN_POINT ( 'NONE',  ( 12.00000000000000533, -5.815948216832730999, -7.788256740848641613 ) ) ;
#21377 = CARTESIAN_POINT ( 'NONE',  ( -14.46758741243234603, -9.725949910454726677, 8.154098604260809680 ) ) ;
#21378 = CARTESIAN_POINT ( 'NONE',  ( -4.062430690931376986, 13.79341706565821291, -4.866449934628417573 ) ) ;
#21379 = FACE_OUTER_BOUND ( 'NONE', #11292, .T. ) ;
#21380 = EDGE_CURVE ( 'NONE', #1857, #1455, #15313, .T. ) ;
#21381 = CARTESIAN_POINT ( 'NONE',  ( -1.963937914100636117, 30.14918992299582712, -0.8991143373722088050 ) ) ;
#21382 = ORIENTED_EDGE ( 'NONE', *, *, #1948, .F. ) ;
#21383 = ADVANCED_FACE ( 'NONE', ( #11328 ), #11465, .T. ) ;
#21384 = CARTESIAN_POINT ( 'NONE',  ( -24.48376588671094822, -1.022231981026950676, 12.50007328825939901 ) ) ;
#21385 = CARTESIAN_POINT ( 'NONE',  ( 24.97017047179999949, -7.684332283202000013, -7.441023909770999367 ) ) ;
#21386 = CARTESIAN_POINT ( 'NONE',  ( 23.07984073068213959, -10.59120176776928268, 0.003446602559681892844 ) ) ;
#21387 = CARTESIAN_POINT ( 'NONE',  ( -20.15132910583999859, -9.188404534074999574, 1.125025998286999896E-14 ) ) ;
#21388 = ORIENTED_EDGE ( 'NONE', *, *, #7893, .T. ) ;
#21389 = CARTESIAN_POINT ( 'NONE',  ( 1.562692578156580359, 24.13277580623734409, -1.623334903882450275 ) ) ;
#21390 = CARTESIAN_POINT ( 'NONE',  ( 0.000000000000000000, 24.39999999221199900, 0.000000000000000000 ) ) ;
#21391 = AXIS2_PLACEMENT_3D ( 'NONE', #9913, #16938, #18646 ) ;
#21392 = DIRECTION ( 'NONE',  ( 0.000000000000000000, 1.000000000000000000, 0.000000000000000000 ) ) ;
#21393 = ORIENTED_EDGE ( 'NONE', *, *, #15088, .F. ) ;
#21394 = CARTESIAN_POINT ( 'NONE',  ( -12.52176908877999928, 6.525220749543999332, -6.187779769309999622 ) ) ;
#21395 = ADVANCED_FACE ( 'NONE', ( #3816 ), #16891, .T. ) ;
#21396 = LINE ( 'NONE', #15322, #12313 ) ;
#21397 = CARTESIAN_POINT ( 'NONE',  ( 2.169242523261438294, 26.43540112775283291, -0.09789572399922988333 ) ) ;
#21398 =( NAMED_UNIT ( * ) PLANE_ANGLE_UNIT ( ) SI_UNIT ( $, .RADIAN. ) );
#21399 = FACE_OUTER_BOUND ( 'NONE', #6577, .T. ) ;
#21400 = ORIENTED_EDGE ( 'NONE', *, *, #15151, .F. ) ;
#21401 = DIRECTION ( 'NONE',  ( 0.9063077870366585964, 0.000000000000000000, 0.4226182617406808451 ) ) ;
#21402 = CARTESIAN_POINT ( 'NONE',  ( 12.67818924931000168, 6.046592098211998945, -8.747551238178997934 ) ) ;
#21403 = CARTESIAN_POINT ( 'NONE',  ( -14.59110758819998743, -8.342498430116506825, -3.617375204252647247 ) ) ;
#21404 = CARTESIAN_POINT ( 'NONE',  ( -20.09640146007999917, -8.409358971373999125, 5.097095819920999027 ) ) ;
#21405 = PLANE ( 'NONE',  #11573 ) ;
#21406 = CARTESIAN_POINT ( 'NONE',  ( 19.86541618412999810, -3.495432200175000226, 8.640661540007000596 ) ) ;
#21407 = CARTESIAN_POINT ( 'NONE',  ( 2.202026052408534440, 28.19497807538909129, 0.1713982358229051983 ) ) ;
#21408 = CARTESIAN_POINT ( 'NONE',  ( 2.817565069457256932, 26.44682129341587995, -2.992080202207100470 ) ) ;
#21409 = ADVANCED_FACE ( 'NONE', ( #13354 ), #7800, .T. ) ;
#21410 = DIRECTION ( 'NONE',  ( 0.000000000000000000, 0.000000000000000000, -1.000000000000000000 ) ) ;
#21411 = ORIENTED_EDGE ( 'NONE', *, *, #11337, .F. ) ;
#21412 = EDGE_CURVE ( 'NONE', #13414, #2324, #21720, .T. ) ;
#21413 = CARTESIAN_POINT ( 'NONE',  ( 2.773360020023811323, 14.06573755500684086, 5.461184526572689713 ) ) ;
#21414 = CARTESIAN_POINT ( 'NONE',  ( 1.332518472557000067, 28.02369850838000076, 1.834054417453000019 ) ) ;
#21415 = AXIS2_PLACEMENT_3D ( 'NONE', #16269, #10946, #12529 ) ;
#21416 = CARTESIAN_POINT ( 'NONE',  ( -19.66003743917331903, 1.201235969070638454, -9.175797021623829153 ) ) ;
#21417 = CARTESIAN_POINT ( 'NONE',  ( -14.50888678659720199, 1.427758690254528950, -8.929076806151241996 ) ) ;
#21418 = CARTESIAN_POINT ( 'NONE',  ( -21.41394528229999850, -11.06275857470000012, 0.7645690033980999667 ) ) ;
#21419 = CARTESIAN_POINT ( 'NONE',  ( 10.35615758860000035, 7.000000000000000000, 0.000000000000000000 ) ) ;
#21420 = CARTESIAN_POINT ( 'NONE',  ( -4.750876579451202453, 12.41232746058178371, 0.9678923958058619492 ) ) ;
#21421 = VERTEX_POINT ( 'NONE', #7683 ) ;
#21422 = PLANE ( 'NONE',  #15709 ) ;
#21423 = CARTESIAN_POINT ( 'NONE',  ( 1.888264321221249542, 11.63400096833999697, -4.433377897947928581 ) ) ;
#21424 = EDGE_CURVE ( 'NONE', #23352, #10646, #18590, .T. ) ;
#21425 = CARTESIAN_POINT ( 'NONE',  ( 0.000000000000000000, 24.65000000000000213, 0.000000000000000000 ) ) ;
#21426 = EDGE_CURVE ( 'NONE', #6143, #8305, #18940, .T. ) ;
#21427 = B_SPLINE_CURVE_WITH_KNOTS ( 'NONE', 3,
 ( #17642, #6247, #6124, #1040, #4810, #12196, #19586, #17152 ),
 .UNSPECIFIED., .F., .F.,
 ( 4, 2, 2, 4 ),
 ( 0.000000000000000000, 0.2500000000000000555, 0.5000000000000000000, 1.000000000000000000 ),
 .UNSPECIFIED. ) ;
#21428 = CARTESIAN_POINT ( 'NONE',  ( 11.69106760960404934, -3.854957646731009380, -8.129799737674142435 ) ) ;
#21429 = B_SPLINE_CURVE_WITH_KNOTS ( 'NONE', 3,
 ( #14394, #21551, #8952, #5198, #3504, #8471, #10772, #23710, #4965, #7116, #17673, #12351, #21900, #3611, #5653, #3724, #7465, #13276, #18272, #14849, #7586, #11115, #9061, #9300, #13041, #16432, #20317, #10994, #18380, #23820, #20204, #12921, #16673, #18499, #20436 ),
 .UNSPECIFIED., .F., .F.,
 ( 4, 1, 1, 1, 1, 1, 1, 1, 1, 1, 1, 1, 1, 1, 1, 1, 1, 1, 1, 1, 1, 1, 1, 1, 1, 1, 1, 1, 1, 1, 1, 1, 4 ),
 ( 0.000000000000000000, 0.01250433631178367658, 0.04500407098468133665, 0.07750380565757906959, 0.1100035403304767956, 0.1425032750033744522, 0.1750030096762721921, 0.2075027443491698487, 0.2400024790222033133, 0.2725022136951010809, 0.3050019483679987098, 0.3375016830408962831, 0.3700014177137940785, 0.4025011523866917629, 0.4350008870595893917, 0.4675006217326229119, 0.5000003564055205407, 0.5325000910784183361, 0.5649998257513160205, 0.5974995604242137048, 0.6299992950971115002, 0.6624990297700089625, 0.6949987644430426492, 0.7274984991159403336, 0.7599982337888380179, 0.7924979684617357023, 0.8249977031346332756, 0.8574974378075309600, 0.8899971724805646467, 0.9224969071534622200, 0.9549966418263599044, 0.9874963764992575888, 1.000000000000000000 ),
 .UNSPECIFIED. ) ;
#21430 = CARTESIAN_POINT ( 'NONE',  ( -2.704962792832999785, 27.25000000000000000, 5.204962792833000229 ) ) ;
#21431 = CARTESIAN_POINT ( 'NONE',  ( -12.50046137836000071, 5.020438948778999766, -14.40607103599000105 ) ) ;
#21432 = CARTESIAN_POINT ( 'NONE',  ( 11.82343232744396921, -8.387570696992149522, -3.192494120993503604 ) ) ;
#21433 = CARTESIAN_POINT ( 'NONE',  ( 12.95437642131000011, -1.177851786523999911, 9.550625374955998836 ) ) ;
#21434 = CARTESIAN_POINT ( 'NONE',  ( -10.34021276376999943, -7.100000000000000533, 0.000000000000000000 ) ) ;
#21435 = EDGE_LOOP ( 'NONE', ( #22574, #1165, #5492, #13541, #14020 ) ) ;
#21436 = CARTESIAN_POINT ( 'NONE',  ( -2.500000000000000000, 28.80000000000000071, 0.000000000000000000 ) ) ;
#21437 = CARTESIAN_POINT ( 'NONE',  ( -2.325054514425000107, 30.26436100756000158, 0.2794086195161999964 ) ) ;
#21438 = CARTESIAN_POINT ( 'NONE',  ( -15.31399577250666688, 4.564820640773371352, 7.920283476814353740 ) ) ;
#21439 = DIRECTION ( 'NONE',  ( 1.000000000000000000, 0.000000000000000000, 0.000000000000000000 ) ) ;
#21440 = ORIENTED_EDGE ( 'NONE', *, *, #7474, .F. ) ;
#21441 = DIRECTION ( 'NONE',  ( 0.000000000000000000, 1.000000000000000000, 0.000000000000000000 ) ) ;
#21442 = CARTESIAN_POINT ( 'NONE',  ( 1.800000000000000044, 12.90000000000000036, -17.04402002421999995 ) ) ;
#21443 = CARTESIAN_POINT ( 'NONE',  ( -24.50000000000000000, -12.50000000001108091, 0.000000000000000000 ) ) ;
#21444 = CARTESIAN_POINT ( 'NONE',  ( -6.042815635770000249, 16.39253429789999927, 0.9999999720525000191 ) ) ;
#21445 = CARTESIAN_POINT ( 'NONE',  ( 14.55941028374722812, 8.833975226579921625, -5.424247256400066775 ) ) ;
#21446 = CARTESIAN_POINT ( 'NONE',  ( 10.35615758860000035, 0.000000000000000000, 7.000000000000000000 ) ) ;
#21447 = CARTESIAN_POINT ( 'NONE',  ( -21.92753743917333864, -9.233985540631776345, -1.208852828397224632 ) ) ;
#21448 = CARTESIAN_POINT ( 'NONE',  ( -23.74465998031000069, -7.716878364870000340, 11.63397459621999985 ) ) ;
#21449 = ORIENTED_EDGE ( 'NONE', *, *, #3894, .F. ) ;
#21450 = CARTESIAN_POINT ( 'NONE',  ( -5.730762473771000565, 28.00000000000000000, 1.577381738259000077 ) ) ;
#21451 = CARTESIAN_POINT ( 'NONE',  ( 11.48696334738999347, -12.46086172551006577, 3.416997251935109059 ) ) ;
#21452 = ORIENTED_EDGE ( 'NONE', *, *, #10996, .T. ) ;
#21453 = CARTESIAN_POINT ( 'NONE',  ( 2.099426398219999879, 25.23106871291000175, -1.438876042424000135 ) ) ;
#21454 = FACE_OUTER_BOUND ( 'NONE', #9954, .T. ) ;
#21455 = CARTESIAN_POINT ( 'NONE',  ( 3.871436389726701233, 13.30584025295970640, 5.593675438725219884 ) ) ;
#21456 = AXIS2_PLACEMENT_3D ( 'NONE', #11925, #19309, #2721 ) ;
#21457 = CARTESIAN_POINT ( 'NONE',  ( 6.188762112849826025, 13.92751971542314138, -0.7696703758847552868 ) ) ;
#21458 = CARTESIAN_POINT ( 'NONE',  ( -6.051726996036002504, 16.51353013550999194, -0.9910466829373008046 ) ) ;
#21459 = CARTESIAN_POINT ( 'NONE',  ( -3.000000000000000000, 20.00000000000000000, 0.000000000000000000 ) ) ;
#21460 = ORIENTED_EDGE ( 'NONE', *, *, #1371, .T. ) ;
#21461 = CARTESIAN_POINT ( 'NONE',  ( -1.259047450927242018, 29.96753006952333465, 2.184465970885648201 ) ) ;
#21462 = CIRCLE ( 'NONE', #4044, 12.89775331292476857 ) ;
#21463 = DIRECTION ( 'NONE',  ( 0.000000000000000000, 1.000000000000000000, 0.000000000000000000 ) ) ;
#21464 = DIRECTION ( 'NONE',  ( 0.000000000000000000, -1.000000000000000000, 0.000000000000000000 ) ) ;
#21465 = EDGE_CURVE ( 'NONE', #8871, #8984, #17988, .T. ) ;
#21466 = VERTEX_POINT ( 'NONE', #20757 ) ;
#21467 = CARTESIAN_POINT ( 'NONE',  ( -21.21750115016000393, 4.272008970125000360, 9.243565099026998411 ) ) ;
#21468 = CARTESIAN_POINT ( 'NONE',  ( 20.98241666666665850, 8.969978628699989187, -2.410745119152057914 ) ) ;
#21469 = CARTESIAN_POINT ( 'NONE',  ( 14.97544413412106756, 10.11390979503470078, 2.113747987315613752 ) ) ;
#21470 = DIRECTION ( 'NONE',  ( -1.000000000000000000, 0.000000000000000000, 0.000000000000000000 ) ) ;
#21471 = CARTESIAN_POINT ( 'NONE',  ( 1.543039561260000081, 29.51287673621999730, 1.780670965265999994 ) ) ;
#21472 = CARTESIAN_POINT ( 'NONE',  ( -22.30014857772672343, -9.241084326725088616, 1.209620885877401131 ) ) ;
#21473 = CARTESIAN_POINT ( 'NONE',  ( -4.719398433761999634, 12.53456689658000656, -0.3214035655570999239 ) ) ;
#21474 = ORIENTED_EDGE ( 'NONE', *, *, #14863, .T. ) ;
#21475 = CARTESIAN_POINT ( 'NONE',  ( -13.64582336266999896, -8.030615239332000499, -7.932400521014000283 ) ) ;
#21476 = CARTESIAN_POINT ( 'NONE',  ( -0.6018193462441471242, 29.56788224182974645, 2.074376258238080251 ) ) ;
#21477 = ORIENTED_EDGE ( 'NONE', *, *, #19169, .T. ) ;
#21478 = CARTESIAN_POINT ( 'NONE',  ( -1.259047450927251566, 29.46666666666666856, -2.184465970885643316 ) ) ;
#21479 = CIRCLE ( 'NONE', #2118, 4.549999999999999822 ) ;
#21480 = CARTESIAN_POINT ( 'NONE',  ( -17.70420214142508541, -10.38169273393352299, 2.154482946468162297 ) ) ;
#21481 = B_SPLINE_CURVE_WITH_KNOTS ( 'NONE', 3,
 ( #10458, #1608, #6806, #1365, #6932, #17847, #21716, #14200 ),
 .UNSPECIFIED., .F., .F.,
 ( 4, 2, 2, 4 ),
 ( 0.000000000000000000, 0.2500000000000000000, 0.5000000000000000000, 1.000000000000000000 ),
 .UNSPECIFIED. ) ;
#21482 = ORIENTED_EDGE ( 'NONE', *, *, #21116, .T. ) ;
#21483 = DIRECTION ( 'NONE',  ( 0.000000000000000000, -1.000000000000000000, 0.000000000000000000 ) ) ;
#21484 = CARTESIAN_POINT ( 'NONE',  ( 4.725397782510998290, 14.52029874379999264, -3.829245615367002031 ) ) ;
#21485 = DIRECTION ( 'NONE',  ( 0.000000000000000000, 1.000000000000000000, 0.000000000000000000 ) ) ;
#21486 = CARTESIAN_POINT ( 'NONE',  ( 15.95626817440999901, -0.1031805989180999972, -11.05505056420000010 ) ) ;
#21487 = CARTESIAN_POINT ( 'NONE',  ( 15.61331408530999987, -8.260803322383997838, -5.986632065681000370 ) ) ;
#21488 = EDGE_LOOP ( 'NONE', ( #4618, #20285, #2667, #21091 ) ) ;
#21489 = CARTESIAN_POINT ( 'NONE',  ( -9.094558992920999785, -6.050585292417999916, -13.19663489122999955 ) ) ;
#21490 = CARTESIAN_POINT ( 'NONE',  ( 4.549999861571000004, 21.99999986157541798, -6.289351278164000247E-08 ) ) ;
#21491 = EDGE_CURVE ( 'NONE', #10829, #15998, #15330, .T. ) ;
#21492 = ORIENTED_EDGE ( 'NONE', *, *, #9766, .T. ) ;
#21493 = CARTESIAN_POINT ( 'NONE',  ( -23.88684722629999868, -8.668318262646000250, -4.424847982898000964 ) ) ;
#21494 = CARTESIAN_POINT ( 'NONE',  ( 11.36701043060024041, 12.20499207204542280, 3.860262462447420440 ) ) ;
#21495 = DIRECTION ( 'NONE',  ( 0.000000000000000000, 1.000000000000000000, 0.000000000000000000 ) ) ;
#21496 = AXIS2_PLACEMENT_3D ( 'NONE', #9933, #13566, #20959 ) ;
#21497 = CARTESIAN_POINT ( 'NONE',  ( 23.99062354302999722, -7.716878364870000340, 11.63397459621999985 ) ) ;
#21498 = CARTESIAN_POINT ( 'NONE',  ( 16.35004977966324446, 2.603377162649796350, -10.05366246871247959 ) ) ;
#21499 = LINE ( 'NONE', #10844, #3666 ) ;
#21500 = DIRECTION ( 'NONE',  ( 0.000000000000000000, -1.000000000000000000, 0.000000000000000000 ) ) ;
#21501 = B_SPLINE_CURVE_WITH_KNOTS ( 'NONE', 3,
 ( #15328, #22719, #14253, #6860, #8447, #4815, #3128, #18138, #23206, #6983, #16052, #12680, #10386, #19946, #20066, #21525, #23445, #1543 ),
 .UNSPECIFIED., .F., .F.,
 ( 4, 2, 2, 2, 2, 2, 2, 2, 4 ),
 ( 0.000000000000000000, 0.1249999999999999167, 0.2499999999999998335, 0.3749999999999998335, 0.4999999999999998890, 0.6249999999999998890, 0.7499999999999998890, 0.8750000000000000000, 1.000000000000000000 ),
 .UNSPECIFIED. ) ;
#21502 = CARTESIAN_POINT ( 'NONE',  ( 1.055729715565287385, 26.42936170367563875, 4.009276318043866638 ) ) ;
#21503 = FACE_OUTER_BOUND ( 'NONE', #21977, .T. ) ;
#21504 = EDGE_CURVE ( 'NONE', #14207, #8305, #14197, .T. ) ;
#21505 = CARTESIAN_POINT ( 'NONE',  ( -1.896736228727305740, 30.14027807355979505, -1.033228027540613381 ) ) ;
#21506 = EDGE_LOOP ( 'NONE', ( #9452, #9999, #11407, #4567 ) ) ;
#21507 = CARTESIAN_POINT ( 'NONE',  ( -2.293740706879999980, 25.43854303844000242, 0.4406523845536999828 ) ) ;
#21508 = CARTESIAN_POINT ( 'NONE',  ( 18.73357886744999945, -4.598493306945000469, 9.790775688502000307 ) ) ;
#21509 = CARTESIAN_POINT ( 'NONE',  ( 22.76773351039173221, -4.982168945016796968, 9.336842154732323706 ) ) ;
#21510 = DIRECTION ( 'NONE',  ( 0.000000000000000000, 1.000000000000000000, 0.000000000000000000 ) ) ;
#21511 = VERTEX_POINT ( 'NONE', #11561 ) ;
#21512 = DIRECTION ( 'NONE',  ( 0.000000000000000000, 1.000000000000000000, 0.000000000000000000 ) ) ;
#21513 = CARTESIAN_POINT ( 'NONE',  ( 5.064386902162485882, 14.06000371052163445, 3.938615721984927820 ) ) ;
#21514 = VECTOR ( 'NONE', #22495, 1000.000000000000000 ) ;
#21515 = CARTESIAN_POINT ( 'NONE',  ( 0.000000000000000000, 18.10000000000000142, 0.000000000000000000 ) ) ;
#21516 = ORIENTED_EDGE ( 'NONE', *, *, #20373, .T. ) ;
#21517 = CARTESIAN_POINT ( 'NONE',  ( -15.28399451769901773, -3.699222542850097550, -9.694524040023539513 ) ) ;
#21518 = DIRECTION ( 'NONE',  ( 0.000000000000000000, -1.000000000000000000, 0.000000000000000000 ) ) ;
#21519 = ORIENTED_EDGE ( 'NONE', *, *, #12532, .F. ) ;
#21520 = LINE ( 'NONE', #10509, #22968 ) ;
#21521 = SHAPE_REPRESENTATION_RELATIONSHIP ( 'NONE' , 'NONE' ,  #20207, #15121 ) ;
#21522 = DIRECTION ( 'NONE',  ( -1.000000000000000000, 0.000000000000000000, 0.000000000000000000 ) ) ;
#21523 = EDGE_CURVE ( 'NONE', #20749, #20574, #4998, .T. ) ;
#21524 = ORIENTED_EDGE ( 'NONE', *, *, #15129, .F. ) ;
#21525 = CARTESIAN_POINT ( 'NONE',  ( -19.47341549180334752, 8.981945570196975481, 2.139161086732093153 ) ) ;
#21526 = CARTESIAN_POINT ( 'NONE',  ( -4.178937961678600210, 15.14834147970980283, -4.478992075710971577 ) ) ;
#21527 = CARTESIAN_POINT ( 'NONE',  ( -19.56251082389000118, -9.430400074637001140, 5.862072811040999198 ) ) ;
#21528 = CARTESIAN_POINT ( 'NONE',  ( -15.89837426871000226, -1.404306094088999979, -10.18324534259000025 ) ) ;
#21529 = CARTESIAN_POINT ( 'NONE',  ( -6.089104266536998544, 16.42834722451999241, 1.007215775395999602 ) ) ;
#21530 = CARTESIAN_POINT ( 'NONE',  ( 16.41181994525999954, -9.662517015497000372, -3.561852019405000291 ) ) ;
#21531 = CARTESIAN_POINT ( 'NONE',  ( 0.000000000000000000, 16.89999999999999858, 0.000000000000000000 ) ) ;
#21532 = AXIS2_PLACEMENT_3D ( 'NONE', #23706, #15172, #13007 ) ;
#21533 = AXIS2_PLACEMENT_3D ( 'NONE', #10422, #8355, #6650 ) ;
#21534 = LINE ( 'NONE', #4948, #17376 ) ;
#21535 = EDGE_CURVE ( 'NONE', #8278, #7192, #22294, .T. ) ;
#21536 = CARTESIAN_POINT ( 'NONE',  ( 15.01133333333333120, -4.561143643790010138, -7.913399690936467223 ) ) ;
#21537 = ORIENTED_EDGE ( 'NONE', *, *, #3047, .F. ) ;
#21538 = CARTESIAN_POINT ( 'NONE',  ( -1.306994031390692035, 26.46241504948189771, -3.864208797664315576 ) ) ;
#21539 = DIRECTION ( 'NONE',  ( 0.000000000000000000, 0.000000000000000000, -1.000000000000000000 ) ) ;
#21540 = CARTESIAN_POINT ( 'NONE',  ( -2.256099604565999783, 27.73119850838000033, -0.2222064166828000287 ) ) ;
#21541 = CARTESIAN_POINT ( 'NONE',  ( 0.5500000000000000444, 1.217911241751999838E-14, 0.000000000000000000 ) ) ;
#21542 = CARTESIAN_POINT ( 'NONE',  ( -14.28497649141528214, 7.354848982022818227, -5.390649801475187353 ) ) ;
#21543 = CARTESIAN_POINT ( 'NONE',  ( -21.74811437386000179, -3.746343007632000344, 10.44678391489000013 ) ) ;
#21544 = CONICAL_SURFACE ( 'NONE', #11476, 9.879748406101001024, 0.7982263333994560339 ) ;
#21545 = CARTESIAN_POINT ( 'NONE',  ( -3.822473297103945455, 12.09266017900104018, 2.961494058630956161 ) ) ;
#21546 = ORIENTED_EDGE ( 'NONE', *, *, #8110, .F. ) ;
#21547 = CARTESIAN_POINT ( 'NONE',  ( -24.12232999016000079, 1.520060141252000183E-14, 0.000000000000000000 ) ) ;
#21548 = CARTESIAN_POINT ( 'NONE',  ( 4.059701995908764793, 12.16834275931829978, -2.635041455870243965 ) ) ;
#21549 = CARTESIAN_POINT ( 'NONE',  ( -10.16272095229482986, 15.91915081437118218, 1.078441560784934250 ) ) ;
#21550 = AXIS2_PLACEMENT_3D ( 'NONE', #5572, #9445, #22395 ) ;
#21551 = CARTESIAN_POINT ( 'NONE',  ( -2.165649008596949088, 30.83057276060822360, 0.005272181257143124418 ) ) ;
#21552 = EDGE_CURVE ( 'NONE', #2832, #12931, #1515, .T. ) ;
#21553 = ADVANCED_FACE ( 'NONE', ( #13721 ), #6337, .F. ) ;
#21554 = CARTESIAN_POINT ( 'NONE',  ( 5.155702020191999857, 13.97328941143999970, -4.008166040501000893 ) ) ;
#21555 = CARTESIAN_POINT ( 'NONE',  ( -14.25243324638999809, -7.716878364870000340, 11.63397459621999985 ) ) ;
#21556 = CARTESIAN_POINT ( 'NONE',  ( 14.27062642131000025, 9.653071988928001446, -0.2951073761277999696 ) ) ;
#21557 = CARTESIAN_POINT ( 'NONE',  ( 24.50000000000000000, 0.000000000000000000, 12.50000000000000000 ) ) ;
#21558 = ORIENTED_EDGE ( 'NONE', *, *, #8171, .F. ) ;
#21559 = CARTESIAN_POINT ( 'NONE',  ( 5.230516336068609107, 13.89302811135363669, 4.095895456715770599 ) ) ;
#21560 = CARTESIAN_POINT ( 'NONE',  ( -0.8187651254961000324, 29.01927641826999960, 2.471853669016999877 ) ) ;
#21561 = CARTESIAN_POINT ( 'NONE',  ( 0.000000000000000000, 0.000000000000000000, 0.000000000000000000 ) ) ;
#21562 = CARTESIAN_POINT ( 'NONE',  ( 4.160050682987502135, 14.52062904459194392, -4.495645836896323466 ) ) ;
#21563 = CIRCLE ( 'NONE', #3761, 13.93375672974000068 ) ;
#21564 = ORIENTED_EDGE ( 'NONE', *, *, #10881, .T. ) ;
#21565 = CARTESIAN_POINT ( 'NONE',  ( -0.5244086596060245631, 26.50000000000000000, -2.383357424156489657 ) ) ;
#21566 = CARTESIAN_POINT ( 'NONE',  ( -24.36724102302906658, -12.10481948363803539, 4.033677606734435983 ) ) ;
#21567 = B_SPLINE_SURFACE_WITH_KNOTS ( 'NONE', 3, 3, ( 
 ( #5894, #15089, #3971, #6134, #9538, #7724, #4449, #2146, #19219, #17039, #22842, #20679, #4088, #682, #11483, #9658, #18859, #10027, #2383, #4326, #2265, #15208, #8089, #22605, #7960, #6014, #15456, #9773, #554, #13399, #4209, #15332, #200, #22721, #6255 ),
 ( #13638, #5784, #7593, #13524, #13167, #19092, #15932, #19719, #3132, #6625, #1050, #3004, #19353, #10263, #2760, #19471, #10389, #10516, #8451, #1180, #4572, #12088, #2880, #17899, #10143, #22961, #13759, #23327, #12450, #1300, #8691, #15818, #14014, #21161, #8573 ),
 ( #4819, #21404, #17781, #17651, #15689, #8324, #6740, #23449, #23209, #806, #12205, #17530, #16055, #5067, #19594, #21654, #6864, #19833, #3246, #14135, #17412, #21291, #21528, #4943, #8206, #924, #12328, #15573, #13888, #11964, #23080, #4703, #1420, #5634, #16300 ),
 ( #21999, #7212, #9159, #8819, #20300, #16179, #10866, #13018, #7099, #20071, #1653, #23582, #6986, #14375, #12900, #12796, #20184, #21769, #5181, #16414, #3594, #9042, #12563, #60, #19949, #8932, #23925, #3702, #3370, #5290, #18019, #12683, #14826, #10748, #16657 ) ),
 .UNSPECIFIED., .F., .F., .F.,
 ( 4, 4 ),
 ( 4, 1, 1, 1, 1, 1, 1, 1, 1, 1, 1, 1, 1, 1, 1, 1, 1, 1, 1, 1, 1, 1, 1, 1, 1, 1, 1, 1, 1, 1, 1, 1, 4 ),
 ( -0.08408083179837000376, 1.084080831798000188 ),
 ( -0.02000000000000000042, 0.01250000000000000069, 0.04499999999999999833, 0.07749999999999999944, 0.1100000000000000006, 0.1424999999999999878, 0.1749999999999999889, 0.2074999999999999900, 0.2399999999999999911, 0.2725000000000000200, 0.3049999999999999933, 0.3375000000000000222, 0.3699999999999999956, 0.4025000000000000244, 0.4349999999999999978, 0.4675000000000000266, 0.5000000000000000000, 0.5324999999999999734, 0.5649999999999999467, 0.5975000000000000311, 0.6300000000000000044, 0.6624999999999999778, 0.6949999999999999512, 0.7275000000000000355, 0.7600000000000000089, 0.7924999999999999822, 0.8249999999999999556, 0.8575000000000000400, 0.8900000000000000133, 0.9224999999999999867, 0.9549999999999999600, 0.9875000000000000444, 1.020000000000000018 ),
 .UNSPECIFIED. ) ;
#21568 = CARTESIAN_POINT ( 'NONE',  ( 15.99391666666666367, 2.377237531314461361, 8.845295767958798905 ) ) ;
#21569 = EDGE_CURVE ( 'NONE', #23889, #23570, #21117, .T. ) ;
#21570 = FACE_OUTER_BOUND ( 'NONE', #13698, .T. ) ;
#21571 = EDGE_CURVE ( 'NONE', #1942, #8248, #7538, .T. ) ;
#21572 = CARTESIAN_POINT ( 'NONE',  ( 15.11695424184799386, 1.968991340098076304, 10.34192823185278343 ) ) ;
#21573 = AXIS2_PLACEMENT_3D ( 'NONE', #15783, #21368, #4785 ) ;
#21574 = CARTESIAN_POINT ( 'NONE',  ( -3.835584729116002123, 14.03840790544035144, 4.850097248418875573 ) ) ;
#21575 = DIRECTION ( 'NONE',  ( 1.000000000000000000, 0.000000000000000000, 0.000000000000000000 ) ) ;
#21576 = CARTESIAN_POINT ( 'NONE',  ( 23.99478584076000232, 13.93375672974000068, -0.6736217021363000157 ) ) ;
#21577 = ORIENTED_EDGE ( 'NONE', *, *, #10251, .T. ) ;
#21578 = CARTESIAN_POINT ( 'NONE',  ( 1.716093532388071496, 30.62679492094257228, 1.703340837445145306 ) ) ;
#21579 = CARTESIAN_POINT ( 'NONE',  ( 1.719784723310866736, 12.95979884212811939, 1.059170354069117970 ) ) ;
#21580 = ORIENTED_EDGE ( 'NONE', *, *, #21491, .F. ) ;
#21581 = CARTESIAN_POINT ( 'NONE',  ( -1.361252172549999973, 24.88271731528999808, 2.150569224523000145 ) ) ;
#21582 = CARTESIAN_POINT ( 'NONE',  ( 5.701363503176997583, 14.61139651266002026, 2.265470104175000721 ) ) ;
#21583 = CARTESIAN_POINT ( 'NONE',  ( 0.8910436668603369803, 12.82851146553231203, 6.615463406976411775 ) ) ;
#21584 = CIRCLE ( 'NONE', #14614, 2.100000000000000089 ) ;
#21585 = CARTESIAN_POINT ( 'NONE',  ( 6.224861414451202890, 13.76529413338021612, -1.291206515654964804 ) ) ;
#21586 = CARTESIAN_POINT ( 'NONE',  ( 66.60588651278291650, 35.51856778792605240, 1.000000000000000000 ) ) ;
#21587 = LINE ( 'NONE', #21459, #4768 ) ;
#21588 = B_SPLINE_CURVE_WITH_KNOTS ( 'NONE', 3,
 ( #12249, #21447, #8493, #17823, #1218, #6418, #15858, #19261, #11759, #13803, #8131, #4861, #15371, #6180, #21201, #23120, #13567, #15496 ),
 .UNSPECIFIED., .F., .F.,
 ( 4, 2, 2, 2, 2, 2, 2, 2, 4 ),
 ( 0.000000000000000000, 0.1250000000000000278, 0.2500000000000000000, 0.3749999999999999445, 0.4999999999999999445, 0.6249999999999998890, 0.7499999999999998890, 0.8750000000000000000, 1.000000000000000000 ),
 .UNSPECIFIED. ) ;
#21589 = EDGE_LOOP ( 'NONE', ( #5307, #9049, #7732, #7219 ) ) ;
#21590 = CARTESIAN_POINT ( 'NONE',  ( 2.500000000000001776, 30.21753006952333109, 0.3272492347489266429 ) ) ;
#21591 = CARTESIAN_POINT ( 'NONE',  ( 13.50000000000000000, 10.65000000000000036, 0.000000000000000000 ) ) ;
#21592 = LINE ( 'NONE', #11898, #8680 ) ;
#21593 = EDGE_LOOP ( 'NONE', ( #10539, #941, #5165, #11542 ) ) ;
#21594 = CARTESIAN_POINT ( 'NONE',  ( -24.37462408469000152, -9.611684602066999261, -4.906288292759999337 ) ) ;
#21595 = CARTESIAN_POINT ( 'NONE',  ( -3.099999776787000005, 16.99999977679100027, -5.570936493763999179E-07 ) ) ;
#21596 = CARTESIAN_POINT ( 'NONE',  ( 15.14795571169218924, 7.213078467210109146, 7.405181219479683108 ) ) ;
#21597 = CARTESIAN_POINT ( 'NONE',  ( -7.500000000000000000, 22.00000000000000000, -1.000000000000000000 ) ) ;
#21598 = CARTESIAN_POINT ( 'NONE',  ( 2.133199474671000129, 30.51333916994999740, -0.3868384114466000279 ) ) ;
#21599 = CARTESIAN_POINT ( 'NONE',  ( -12.25000000000000000, 1.374666032043000015E-14, 0.000000000000000000 ) ) ;
#21600 = CARTESIAN_POINT ( 'NONE',  ( 4.721486246517997643, 12.60723799037000070, -0.5132971997070995274 ) ) ;
#21601 = ORIENTED_EDGE ( 'NONE', *, *, #10771, .F. ) ;
#21602 = CARTESIAN_POINT ( 'NONE',  ( -23.74228231688656976, 8.693394395448456762E-05, -9.522797051439189531 ) ) ;
#21603 = CARTESIAN_POINT ( 'NONE',  ( -0.2387898408332101985, 29.21801578594281068, -2.146576094895672693 ) ) ;
#21604 = ORIENTED_EDGE ( 'NONE', *, *, #11058, .F. ) ;
#21605 = LINE ( 'NONE', #3201, #7230 ) ;
#21606 = CARTESIAN_POINT ( 'NONE',  ( -14.49195384425397215, 0.7433570823107922276, 10.32670728092745804 ) ) ;
#21607 = ORIENTED_EDGE ( 'NONE', *, *, #20329, .F. ) ;
#21608 = AXIS2_PLACEMENT_3D ( 'NONE', #17691, #10061, #12001 ) ;
#21609 = CARTESIAN_POINT ( 'NONE',  ( 0.000000000000000000, -1.550000000000000044, 0.000000000000000000 ) ) ;
#21610 = CARTESIAN_POINT ( 'NONE',  ( 16.71195833333331748, -7.277172784690141505, -5.592373574543976211 ) ) ;
#21611 = CARTESIAN_POINT ( 'NONE',  ( 11.99999999999999645, -4.526363629865546301, -7.766451825080983085 ) ) ;
#21612 = AXIS2_PLACEMENT_3D ( 'NONE', #3540, #10923, #9101 ) ;
#21613 = CARTESIAN_POINT ( 'NONE',  ( 16.49762086794999760, 10.59225851661000206, 3.218213586410000104 ) ) ;
#21614 = CARTESIAN_POINT ( 'NONE',  ( 12.10331408531000008, -5.154040300995999857, -8.697259314724000490 ) ) ;
#21615 = ORIENTED_EDGE ( 'NONE', *, *, #8110, .T. ) ;
#21616 = CARTESIAN_POINT ( 'NONE',  ( -9.501848992921001269, -12.26021964927999974, 7.774810108354999194 ) ) ;
#21617 = CARTESIAN_POINT ( 'NONE',  ( -24.50000000000000000, -7.216878364870000340, -12.50000000000000000 ) ) ;
#21618 =( NAMED_UNIT ( * ) SI_UNIT ( $, .STERADIAN. ) SOLID_ANGLE_UNIT ( ) );
#21619 = VERTEX_POINT ( 'NONE', #20882 ) ;
#21620 = FACE_OUTER_BOUND ( 'NONE', #1296, .T. ) ;
#21621 = CARTESIAN_POINT ( 'NONE',  ( 21.44098906717976405, -2.902397506967778096, -10.31605076386551545 ) ) ;
#21622 = CARTESIAN_POINT ( 'NONE',  ( 11.00000000000000000, 0.000000000000000000, 0.000000000000000000 ) ) ;
#21623 = CARTESIAN_POINT ( 'NONE',  ( 16.27506522991737725, -0.06060872261240779491, -10.36580276523552158 ) ) ;
#21624 = CARTESIAN_POINT ( 'NONE',  ( -6.020246122619357543, 14.94718218489679451, 3.809753413873187888 ) ) ;
#21625 = CIRCLE ( 'NONE', #22376, 2.000000000000000000 ) ;
#21626 = CARTESIAN_POINT ( 'NONE',  ( 2.207687974961999977, 29.05785630726000335, -0.7846283158615999787 ) ) ;
#21627 = AXIS2_PLACEMENT_3D ( 'NONE', #10526, #17910, #4713 ) ;
#21628 = CARTESIAN_POINT ( 'NONE',  ( 0.000000000000000000, 26.20000000000000284, 4.618802153517000519 ) ) ;
#21629 = CARTESIAN_POINT ( 'NONE',  ( -1.194153984485240683, 30.07849839638842226, -1.799745786739597619 ) ) ;
#21630 = VERTEX_POINT ( 'NONE', #9974 ) ;
#21631 = CARTESIAN_POINT ( 'NONE',  ( 12.52688711657000020, 13.93375672974000068, -0.8660254037843999608 ) ) ;
#21632 = CARTESIAN_POINT ( 'NONE',  ( 24.47013653015837775, -1.097897350813762829, 10.57183604653516440 ) ) ;
#21633 = CARTESIAN_POINT ( 'NONE',  ( -1.894956018450759005, 23.61932460823316404, -0.9647289121299874592 ) ) ;
#21634 = VECTOR ( 'NONE', #10940, 1000.000000000000000 ) ;
#21635 = VERTEX_POINT ( 'NONE', #8165 ) ;
#21636 = EDGE_CURVE ( 'NONE', #3348, #20171, #22679, .T. ) ;
#21637 = CARTESIAN_POINT ( 'NONE',  ( 24.50000000000000000, -10.82531754731000007, -6.250000000000000000 ) ) ;
#21638 = CYLINDRICAL_SURFACE ( 'NONE', #10816, 3.000000000000002665 ) ;
#21639 = CARTESIAN_POINT ( 'NONE',  ( -4.024865567630999230, 12.19225766109002329, -2.884015414602999705 ) ) ;
#21640 = EDGE_LOOP ( 'NONE', ( #18131, #10582 ) ) ;
#21641 = AXIS2_PLACEMENT_3D ( 'NONE', #16440, #3512, #10893 ) ;
#21642 = CARTESIAN_POINT ( 'NONE',  ( 17.20575125731000199, -0.07625726307336000431, -9.225306777752001253 ) ) ;
#21643 = EDGE_LOOP ( 'NONE', ( #917, #19368, #12871, #2227 ) ) ;
#21644 = CIRCLE ( 'NONE', #1921, 15.43375672974000068 ) ;
#21645 = CARTESIAN_POINT ( 'NONE',  ( -14.00000000000000000, 1.396097351027999937E-14, 0.000000000000000000 ) ) ;
#21646 = CONTEXT_DEPENDENT_SHAPE_REPRESENTATION ( #18399, #13446 ) ;
#21647 = CARTESIAN_POINT ( 'NONE',  ( -14.42499035157127985, -3.357933904613944254, -12.49997221285484983 ) ) ;
#21648 = EDGE_CURVE ( 'NONE', #22330, #611, #881, .T. ) ;
#21649 = EDGE_LOOP ( 'NONE', ( #2499, #20119, #7081, #8894, #22502 ) ) ;
#21650 = CARTESIAN_POINT ( 'NONE',  ( 0.5031143267968901656, 26.62499557077888213, 2.497567878996554747 ) ) ;
#21651 = CIRCLE ( 'NONE', #3088, 2.899999999999999911 ) ;
#21652 = CARTESIAN_POINT ( 'NONE',  ( 12.23943924931000105, -8.418214415862998123, -6.478404025908999664 ) ) ;
#21653 = CARTESIAN_POINT ( 'NONE',  ( -21.11638508900000133, -3.075672562904000262, -10.17210945827999957 ) ) ;
#21654 = CARTESIAN_POINT ( 'NONE',  ( -17.32028670448999819, 9.694482879840998990, -3.536072490757000253 ) ) ;
#21655 = CARTESIAN_POINT ( 'NONE',  ( -0.8491321808595133636, 24.60222989789001957, 4.128541458487867466 ) ) ;
#21656 = CARTESIAN_POINT ( 'NONE',  ( -24.24164425323710503, 6.933586358082536982, -8.021408670079015479 ) ) ;
#21657 = CARTESIAN_POINT ( 'NONE',  ( 0.9780573793134281768, 28.06247231623991212, 1.979757165466330626 ) ) ;
#21658 = DIRECTION ( 'NONE',  ( -1.000000000000000000, 0.000000000000000000, 0.000000000000000000 ) ) ;
#21659 = VECTOR ( 'NONE', #23816, 1000.000000000000000 ) ;
#21660 = CARTESIAN_POINT ( 'NONE',  ( 0.000000000000000000, 19.09999999999999787, -3.000000000003983480 ) ) ;
#21661 = ORIENTED_EDGE ( 'NONE', *, *, #22955, .T. ) ;
#21662 = CARTESIAN_POINT ( 'NONE',  ( 23.33304596532290276, 7.619942348972831070, 5.313059321050398687 ) ) ;
#21663 = FACE_OUTER_BOUND ( 'NONE', #1536, .T. ) ;
#21664 = CARTESIAN_POINT ( 'NONE',  ( 1.206163983883000057, 25.98413313894999987, -2.153772461420000006 ) ) ;
#21665 = ADVANCED_FACE ( 'NONE', ( #2717 ), #8410, .T. ) ;
#21666 = CARTESIAN_POINT ( 'NONE',  ( 5.982801910263268574, 14.41040939236866514, -1.321542980959287794 ) ) ;
#21667 = CARTESIAN_POINT ( 'NONE',  ( 1.439795436514999860, 28.09437716036000410, 1.981708497821000226 ) ) ;
#21668 = CARTESIAN_POINT ( 'NONE',  ( -4.850001362640682601, 12.45000000000000284, 0.1690184008927609061 ) ) ;
#21669 = VERTEX_POINT ( 'NONE', #10219 ) ;
#21670 = CARTESIAN_POINT ( 'NONE',  ( 0.000000000000000000, -1.550000000000000044, 0.000000000000000000 ) ) ;
#21671 = CARTESIAN_POINT ( 'NONE',  ( 3.061958301202284627, 11.87766433303262126, -3.731442317003270226 ) ) ;
#21672 = CARTESIAN_POINT ( 'NONE',  ( -7.500000000000000000, 22.00000000000000000, 1.000000000000000000 ) ) ;
#21673 = CARTESIAN_POINT ( 'NONE',  ( -20.75009587121333254, -4.635310582250941280, 8.042080427403897502 ) ) ;
#21674 = VERTEX_POINT ( 'NONE', #6586 ) ;
#21675 = EDGE_CURVE ( 'NONE', #5630, #9908, #7840, .T. ) ;
#21676 = CARTESIAN_POINT ( 'NONE',  ( -2.133997843432942521, 30.69809435506457262, -0.8888301093114056028 ) ) ;
#21677 = CARTESIAN_POINT ( 'NONE',  ( -17.50529997408999705, -11.39253675243999986, 0.2566028257674999868 ) ) ;
#21678 = CARTESIAN_POINT ( 'NONE',  ( 14.59968892130999940, 4.304969983318999383, 8.654667617400001234 ) ) ;
#21679 = CARTESIAN_POINT ( 'NONE',  ( 18.70390242685546411, 8.868690283753592141, 5.485530365214523307 ) ) ;
#21680 = ORIENTED_EDGE ( 'NONE', *, *, #22345, .F. ) ;
#21681 = DIRECTION ( 'NONE',  ( 0.000000000000000000, 1.000000000000000000, 0.000000000000000000 ) ) ;
#21682 = CARTESIAN_POINT ( 'NONE',  ( 0.2733293520537999899, 30.56833479956000232, 2.518019340826000096 ) ) ;
#21683 = CARTESIAN_POINT ( 'NONE',  ( 2.593577339411000438, 23.81257639262999959, -0.8064155041328999740 ) ) ;
#21684 = CARTESIAN_POINT ( 'NONE',  ( 13.49999999999999645, -9.465184455976315192, 2.727039375416640876 ) ) ;
#21685 = EDGE_LOOP ( 'NONE', ( #14701, #3122, #15670, #14482, #9686 ) ) ;
#21686 = EDGE_CURVE ( 'NONE', #13042, #21878, #18445, .T. ) ;
#21687 = CARTESIAN_POINT ( 'NONE',  ( 6.124999911758999716, 14.37502625872000195, -0.0001546258496581000123 ) ) ;
#21688 = CARTESIAN_POINT ( 'NONE',  ( 0.000000000000000000, -1.550000000000000044, 0.000000000000000000 ) ) ;
#21689 = FACE_OUTER_BOUND ( 'NONE', #13632, .T. ) ;
#21690 = CARTESIAN_POINT ( 'NONE',  ( -0.6074916215089999350, 30.83999999999999986, -2.072813047478000215 ) ) ;
#21691 = CARTESIAN_POINT ( 'NONE',  ( 14.30851550260190663, 1.558156080228414009, -10.24440842901224080 ) ) ;
#21692 = CARTESIAN_POINT ( 'NONE',  ( -4.008718708443686829, 13.84443620156353383, 4.855404245198969626 ) ) ;
#21693 = CARTESIAN_POINT ( 'NONE',  ( -4.550974324282003103, 12.30365742415998831, 1.872281734269997999 ) ) ;
#21694 = ADVANCED_FACE ( 'NONE', ( #14563 ), #15178, .F. ) ;
#21695 = DIRECTION ( 'NONE',  ( 1.000000000000000000, 0.000000000000000000, 0.000000000000000000 ) ) ;
#21696 = ORIENTED_EDGE ( 'NONE', *, *, #21686, .T. ) ;
#21697 = DIRECTION ( 'NONE',  ( 1.511005137241999593E-08, -0.9999999999999997780, 8.997177532459998026E-09 ) ) ;
#21698 = ADVANCED_FACE ( 'NONE', ( #9826 ), #2687, .F. ) ;
#21699 = CARTESIAN_POINT ( 'NONE',  ( -8.099999999999999645, 10.50000000000000000, 1.882604183655999859E-09 ) ) ;
#21700 = ORIENTED_EDGE ( 'NONE', *, *, #22451, .T. ) ;
#21701 = CARTESIAN_POINT ( 'NONE',  ( -2.051653534209000096, 24.15210859155000023, 1.811817559062000038 ) ) ;
#21702 = CARTESIAN_POINT ( 'NONE',  ( 6.046348537316000638, 14.51594544156001731, 1.039485355375998843 ) ) ;
#21703 = CARTESIAN_POINT ( 'NONE',  ( 11.90008533511925570, 4.641570061506223865, -12.50003962888440867 ) ) ;
#21704 = CARTESIAN_POINT ( 'NONE',  ( 30.87226923053214378, 27.01856778792605240, 0.000000000000000000 ) ) ;
#21705 = CARTESIAN_POINT ( 'NONE',  ( 13.49999999999999822, -3.814422028142153920, 9.637201378805430707 ) ) ;
#21706 = CARTESIAN_POINT ( 'NONE',  ( 23.41677564524290744, 35.51856778792605240, 6.000000000000000000 ) ) ;
#21707 = EDGE_CURVE ( 'NONE', #9729, #18970, #7216, .T. ) ;
#21708 = VERTEX_POINT ( 'NONE', #20854 ) ;
#21709 = DIRECTION ( 'NONE',  ( -0.000000000000000000, 1.000000000000000000, 0.000000000000000000 ) ) ;
#21710 = CARTESIAN_POINT ( 'NONE',  ( -14.00000000000000000, 15.45000000000000107, 0.000000000000000000 ) ) ;
#21711 = DIRECTION ( 'NONE',  ( 1.000000000000000000, 0.000000000000000000, 0.000000000000000000 ) ) ;
#21712 = ORIENTED_EDGE ( 'NONE', *, *, #973, .F. ) ;
#21713 = CARTESIAN_POINT ( 'NONE',  ( -20.77592263693000163, -9.968135545850000057, -3.872507180638000257 ) ) ;
#21714 = DIRECTION ( 'NONE',  ( 0.000000000000000000, 0.000000000000000000, -1.000000000000000000 ) ) ;
#21715 = CARTESIAN_POINT ( 'NONE',  ( 14.88795491433943141, 10.27596259119593469, -1.066310422897988053 ) ) ;
#21716 = CARTESIAN_POINT ( 'NONE',  ( 4.000000000000071942, 24.70197603011810372, 1.905018119031321566 ) ) ;
#21717 = CARTESIAN_POINT ( 'NONE',  ( 23.17123256445000123, -6.909033356756999922, -8.914582262144000069 ) ) ;
#21718 = CARTESIAN_POINT ( 'NONE',  ( 0.1373810394097000065, 30.19247788257999687, 2.356548280181000266 ) ) ;
#21719 = LINE ( 'NONE', #15882, #6166 ) ;
#21720 = B_SPLINE_CURVE_WITH_KNOTS ( 'NONE', 3,
 ( #22566, #279, #163, #4049 ),
 .UNSPECIFIED., .F., .F.,
 ( 4, 4 ),
 ( 0.000000000000000000, 0.2414086770563061979 ),
 .UNSPECIFIED. ) ;
#21721 = CARTESIAN_POINT ( 'NONE',  ( 0.3622508839787001444, 11.63016099405998816, -4.759913996260000779 ) ) ;
#21722 = ORIENTED_EDGE ( 'NONE', *, *, #9802, .F. ) ;
#21723 = DIRECTION ( 'NONE',  ( 0.000000000000000000, -1.000000000000000000, 0.000000000000000000 ) ) ;
#21724 = ORIENTED_EDGE ( 'NONE', *, *, #18134, .T. ) ;
#21725 = DIRECTION ( 'NONE',  ( -1.000000000000000000, 0.000000000000000000, 0.000000000000000000 ) ) ;
#21726 = PLANE ( 'NONE',  #1099 ) ;
#21727 = ORIENTED_EDGE ( 'NONE', *, *, #14895, .F. ) ;
#21728 = DIRECTION ( 'NONE',  ( 0.000000000000000000, -1.000000000000000000, 0.000000000000000000 ) ) ;
#21729 = FACE_OUTER_BOUND ( 'NONE', #12835, .T. ) ;
#21730 = DIRECTION ( 'NONE',  ( 1.000000000000000000, 0.000000000000000000, 0.000000000000000000 ) ) ;
#21731 = CARTESIAN_POINT ( 'NONE',  ( 17.39987535718000089, -10.66748124715000046, -3.050476693690000296 ) ) ;
#21732 = EDGE_CURVE ( 'NONE', #7192, #15097, #18820, .T. ) ;
#21733 = EDGE_LOOP ( 'NONE', ( #8653, #5792, #20544, #364 ) ) ;
#21734 = CARTESIAN_POINT ( 'NONE',  ( -11.64012149292000053, 14.44913244472000002, -1.408148137578000059 ) ) ;
#21735 = B_SPLINE_CURVE_WITH_KNOTS ( 'NONE', 3,
 ( #20609, #11412, #6188, #18785, #10073 ),
 .UNSPECIFIED., .F., .F.,
 ( 4, 1, 4 ),
 ( 0.000000000000000000, 0.5000000000000000000, 1.000000000000000000 ),
 .UNSPECIFIED. ) ;
#21736 = CYLINDRICAL_SURFACE ( 'NONE', #5137, 2.500000000000000000 ) ;
#21737 = EDGE_LOOP ( 'NONE', ( #15986, #18814, #4758, #1756 ) ) ;
#21738 = CARTESIAN_POINT ( 'NONE',  ( 11.32654380052929532, 12.11008572906302660, 4.024656720653348785 ) ) ;
#21739 = CARTESIAN_POINT ( 'NONE',  ( 20.91152651491986703, -9.035863455013506851, 5.423255042272778326 ) ) ;
#21740 = CARTESIAN_POINT ( 'NONE',  ( -14.00000000000000178, 4.694743687854951553, 8.221477620564558109 ) ) ;
#21741 = CARTESIAN_POINT ( 'NONE',  ( 16.27872609588940023, 0.07001526935372526239, -10.36642397399645255 ) ) ;
#21742 = CARTESIAN_POINT ( 'NONE',  ( -18.62749591150999962, 2.262565266096000283, -10.88529173890999857 ) ) ;
#21743 = AXIS2_PLACEMENT_3D ( 'NONE', #648, #17249, #18827 ) ;
#21744 = CARTESIAN_POINT ( 'NONE',  ( -1.897333882707999964, 30.29912746140999857, 1.090302715689999813 ) ) ;
#21745 = CARTESIAN_POINT ( 'NONE',  ( -18.39867747026000089, -7.918532069388001027, -5.797808426274999150 ) ) ;
#21746 = CARTESIAN_POINT ( 'NONE',  ( 1.535128497521570434, 29.90306122052386328, -1.519513479630941966 ) ) ;
#21747 = ORIENTED_EDGE ( 'NONE', *, *, #11448, .T. ) ;
#21748 = CARTESIAN_POINT ( 'NONE',  ( -23.86847083086815147, -5.679235826686364064, 12.50000000000278533 ) ) ;
#21749 = CARTESIAN_POINT ( 'NONE',  ( 23.81066487044000013, 11.42980371577000120, -1.209163809909999943 ) ) ;
#21750 = CARTESIAN_POINT ( 'NONE',  ( 4.000024251878890880, 28.02555747447231127, -0.7498250608958110242 ) ) ;
#21751 = CARTESIAN_POINT ( 'NONE',  ( -12.25000000000000000, 15.45000000000000107, 0.000000000000000000 ) ) ;
#21752 = ORIENTED_EDGE ( 'NONE', *, *, #2874, .F. ) ;
#21753 = CARTESIAN_POINT ( 'NONE',  ( -4.900699999999999612, 1.284663064832999817E-14, 0.000000000000000000 ) ) ;
#21754 = CARTESIAN_POINT ( 'NONE',  ( 0.000000000000000000, 26.34999999328000087, 0.000000000000000000 ) ) ;
#21755 = CARTESIAN_POINT ( 'NONE',  ( -3.242527372584000034, 11.89078663977000616, -3.603690374931001195 ) ) ;
#21756 = VERTEX_POINT ( 'NONE', #489 ) ;
#21757 = CARTESIAN_POINT ( 'NONE',  ( -6.042815832213999983, 16.39253418350000047, -0.9999999878869999526 ) ) ;
#21758 = ORIENTED_EDGE ( 'NONE', *, *, #3923, .T. ) ;
#21759 = AXIS2_PLACEMENT_3D ( 'NONE', #3914, #5840, #16982 ) ;
#21760 = DIRECTION ( 'NONE',  ( 0.000000000000000000, 0.8660254037844288266, -0.5000000000000169864 ) ) ;
#21761 = SHAPE_DEFINITION_REPRESENTATION ( #689, #12781 ) ;
#21762 = FACE_OUTER_BOUND ( 'NONE', #22950, .T. ) ;
#21763 = B_SPLINE_SURFACE_WITH_KNOTS ( 'NONE', 3, 3, ( 
 ( #3435, #19784, #10693, #3193, #5243, #14436, #10819, #21598, #16120, #18315, #8632, #7276, #18084, #1241, #1489, #10575, #1717, #12854, #3313, #23646, #7053, #15995, #5014, #8756, #6808, #9107, #23756, #8883, #22064, #17962, #10929, #20250, #6934, #21831, #16479 ),
 ( #20013, #3656, #1610, #14549, #8996, #21944, #23390, #1366, #23521, #14330, #21718, #5129, #19896, #20486, #2068, #12, #7396, #9222, #13315, #13202, #20595, #22174, #16602, #16833, #4004, #9459, #14778, #472, #1836, #9340, #358, #20713, #5585, #5701, #18426 ),
 ( #12967, #7511, #18896, #20363, #13087, #3893, #236, #3773, #11161, #18547, #1954, #5930, #7640, #16713, #2306, #22412, #124, #11284, #14894, #5820, #18661, #15013, #13436, #22285, #11402, #7759, #18770, #4121, #2180, #9573, #11518, #16959, #15125, #17074, #22522 ),
 ( #9693, #7875, #15243, #22635, #6047, #20838, #11042, #2539, #2917, #4361, #23116, #2797, #19127, #17567, #23242, #4736, #21321, #19257, #839, #17194, #19385, #13561, #8488, #6176, #15728, #15853, #17316, #2670, #12122, #10179, #22996, #15492, #13926, #9930, #7993 ) ),
 .UNSPECIFIED., .F., .F., .F.,
 ( 4, 4 ),
 ( 4, 1, 1, 1, 1, 1, 1, 1, 1, 1, 1, 1, 1, 1, 1, 1, 1, 1, 1, 1, 1, 1, 1, 1, 1, 1, 1, 1, 1, 1, 1, 1, 4 ),
 ( -0.3056682515952000023, 1.305668251594999996 ),
 ( 0.2487685814243000004, 0.2727048766240999789, 0.2966411718237999540, 0.3205774670234999846, 0.3445137622232000152, 0.3684500574228999903, 0.3923863526226000209, 0.4163226478222999960, 0.4402589430221000022, 0.4641952382218000328, 0.4881315334215000079, 0.5120678286211999275, 0.5360041238209000136, 0.5599404190205999887, 0.5838767142202999638, 0.6078130094200999700, 0.6317493046197999451, 0.6556855998195000312, 0.6796218950192000063, 0.7035581902188999814, 0.7274944854186000676, 0.7514307806182999316, 0.7753670758181000489, 0.7993033710178000240, 0.8232396662174999991, 0.8471759614172000852, 0.8711122566168999493, 0.8950485518166000354, 0.9189848470164000416, 0.9429211422161000167, 0.9668574374157999918, 0.9907937326154999669, 1.014730027814999991 ),
 .UNSPECIFIED. ) ;
#21764 = ORIENTED_EDGE ( 'NONE', *, *, #19470, .F. ) ;
#21765 = CARTESIAN_POINT ( 'NONE',  ( -0.9692852216071858873, 26.54999367254126597, 2.356152689279187307 ) ) ;
#21766 = CARTESIAN_POINT ( 'NONE',  ( -3.711347484313542999, 14.46588732160023483, -4.873238578355667983 ) ) ;
#21767 = CARTESIAN_POINT ( 'NONE',  ( -21.75873182887000112, -6.211188989293999541, 8.644182252947999245 ) ) ;
#21768 = EDGE_CURVE ( 'NONE', #12558, #12473, #16116, .T. ) ;
#21769 = CARTESIAN_POINT ( 'NONE',  ( -17.18320679392000017, 4.803081678427999712, 8.519217971866998695 ) ) ;
#21770 = CARTESIAN_POINT ( 'NONE',  ( -5.666264227037997259, 14.58672067372999770, -4.744312203209001488 ) ) ;
#21771 = CARTESIAN_POINT ( 'NONE',  ( -23.54679585804987951, 0.2324833852550877988, 10.57975454153479866 ) ) ;
#21772 = CARTESIAN_POINT ( 'NONE',  ( 1.126663271959915225, 26.47240320403346558, 1.894978555737950154 ) ) ;
#21773 = CARTESIAN_POINT ( 'NONE',  ( -2.254705796085000102, 28.14500240010000098, 1.777466727206999941 ) ) ;
#21774 = CARTESIAN_POINT ( 'NONE',  ( 1.065127663449546791, 30.73828402243652391, -1.880807996640347701 ) ) ;
#21775 = EDGE_LOOP ( 'NONE', ( #12375, #23597, #21712, #4854 ) ) ;
#21776 = CARTESIAN_POINT ( 'NONE',  ( 23.86147274828209675, -7.124683383478932264, 6.063353310551788056 ) ) ;
#21777 = CARTESIAN_POINT ( 'NONE',  ( -2.270871215252209030, 19.00000000000000000, 0.000000000000000000 ) ) ;
#21778 = CARTESIAN_POINT ( 'NONE',  ( -1.876963106047000007, 26.95913313895000130, -1.603077936557000038 ) ) ;
#21779 = AXIS2_PLACEMENT_3D ( 'NONE', #7749, #9213, #16592 ) ;
#21780 = CARTESIAN_POINT ( 'NONE',  ( 1.117936111508999852, 25.96771896306000116, -1.996229403933999835 ) ) ;
#21781 = CARTESIAN_POINT ( 'NONE',  ( -3.166937750419610342, 11.90469789891420760, 3.644469328947587350 ) ) ;
#21782 = ORIENTED_EDGE ( 'NONE', *, *, #16471, .T. ) ;
#21783 = CARTESIAN_POINT ( 'NONE',  ( -6.000000000000000000, 26.50000000000000000, -6.000000000000000000 ) ) ;
#21784 = CARTESIAN_POINT ( 'NONE',  ( 4.632870948126061705, 12.36824807791137104, -1.431490575886223748 ) ) ;
#21785 = CARTESIAN_POINT ( 'NONE',  ( 1.547047946228873982, 6.951972372782297072, 0.8197927924581556169 ) ) ;
#21786 = ORIENTED_EDGE ( 'NONE', *, *, #16624, .F. ) ;
#21787 = CARTESIAN_POINT ( 'NONE',  ( 6.125000000000000000, 21.50000000000000000, 0.000000000000000000 ) ) ;
#21788 = CARTESIAN_POINT ( 'NONE',  ( -10.90000000000000036, 1.358133300253999998E-14, 0.000000000000000000 ) ) ;
#21789 = DIRECTION ( 'NONE',  ( -3.842525697690999187E-09, -0.9999999999999998890, 1.654014171407999877E-08 ) ) ;
#21790 = CARTESIAN_POINT ( 'NONE',  ( 16.79343892131000260, -7.329510781495000238, 6.390029238976000059 ) ) ;
#21791 = CARTESIAN_POINT ( 'NONE',  ( 18.81675108960719456, 6.131865051825325708, 8.439018125457318220 ) ) ;
#21792 = EDGE_CURVE ( 'NONE', #3147, #17, #6994, .T. ) ;
#21793 = ORIENTED_EDGE ( 'NONE', *, *, #13937, .F. ) ;
#21794 = CYLINDRICAL_SURFACE ( 'NONE', #11195, 2.100000000000000089 ) ;
#21795 = DIRECTION ( 'NONE',  ( 0.000000000000000000, 1.000000000000000000, 0.000000000000000000 ) ) ;
#21796 = CARTESIAN_POINT ( 'NONE',  ( -12.50116661936999840, 6.705358320533000516, -5.997050322680999912 ) ) ;
#21797 = CARTESIAN_POINT ( 'NONE',  ( 13.50000000000000355, -6.133804904974399008, 8.162014436799776007 ) ) ;
#21798 = VERTEX_POINT ( 'NONE', #14187 ) ;
#21799 = FACE_OUTER_BOUND ( 'NONE', #10151, .T. ) ;
#21800 = CARTESIAN_POINT ( 'NONE',  ( 0.000000000000000000, 17.89999999999999858, 0.000000000000000000 ) ) ;
#21801 = DIRECTION ( 'NONE',  ( 1.000000000000000000, 0.000000000000000000, 0.000000000000000000 ) ) ;
#21802 = CARTESIAN_POINT ( 'NONE',  ( 13.50000000000000000, -4.865356088987999428, 9.073685197596999430 ) ) ;
#21803 = FACE_OUTER_BOUND ( 'NONE', #22978, .T. ) ;
#21804 = CARTESIAN_POINT ( 'NONE',  ( -4.101460439749002873, 12.21661303934001097, 2.777632186137001913 ) ) ;
#21805 = ADVANCED_FACE ( 'NONE', ( #7144 ), #6844, .T. ) ;
#21806 = CARTESIAN_POINT ( 'NONE',  ( -19.47031957961999638, -4.572788659038001136, 10.04465920712000049 ) ) ;
#21807 = VERTEX_POINT ( 'NONE', #10562 ) ;
#21808 = CARTESIAN_POINT ( 'NONE',  ( -14.65021834701999204, -8.903882834198213914, -1.852295623008597625 ) ) ;
#21809 = CARTESIAN_POINT ( 'NONE',  ( 1.739740853794686792, 12.98133831228224899, 1.064828544757462137 ) ) ;
#21810 = ORIENTED_EDGE ( 'NONE', *, *, #11754, .T. ) ;
#21811 = CARTESIAN_POINT ( 'NONE',  ( 2.541521031844999889, 25.16139843338999782, -0.1364782455292000152 ) ) ;
#21812 = DIRECTION ( 'NONE',  ( 0.000000000000000000, 0.000000000000000000, -1.000000000000000000 ) ) ;
#21813 = CARTESIAN_POINT ( 'NONE',  ( 11.18529249867571806, 1.746922494874735499, -12.50002083036462430 ) ) ;
#21814 = AXIS2_PLACEMENT_3D ( 'NONE', #17245, #2114, #22925 ) ;
#21815 = DIRECTION ( 'NONE',  ( 0.000000000000000000, 1.000000000000000000, 0.000000000000000000 ) ) ;
#21816 = CARTESIAN_POINT ( 'NONE',  ( 2.100000000000000089, 18.00000000000000000, 0.000000000000000000 ) ) ;
#21817 = EDGE_CURVE ( 'NONE', #12435, #20353, #4370, .T. ) ;
#21818 = FACE_OUTER_BOUND ( 'NONE', #8405, .T. ) ;
#21819 = ORIENTED_EDGE ( 'NONE', *, *, #17867, .F. ) ;
#21820 = FACE_OUTER_BOUND ( 'NONE', #13579, .T. ) ;
#21821 = DIRECTION ( 'NONE',  ( 0.000000000000000000, 1.000000000000000000, 0.000000000000000000 ) ) ;
#21822 = DIRECTION ( 'NONE',  ( 0.000000000000000000, 1.000000000000000000, 0.000000000000000000 ) ) ;
#21823 = EDGE_CURVE ( 'NONE', #837, #10482, #7282, .T. ) ;
#21824 = EDGE_LOOP ( 'NONE', ( #19330, #23543, #15074, #7951, #77, #22189 ) ) ;
#21825 = CARTESIAN_POINT ( 'NONE',  ( -19.23362201646000003, -8.964731209158999903, 5.752370880095000416 ) ) ;
#21826 = CARTESIAN_POINT ( 'NONE',  ( 2.104585786644999956, 25.66586702996999847, 0.4122421647189999927 ) ) ;
#21827 = CARTESIAN_POINT ( 'NONE',  ( 14.54008231524181483, 2.694371657221933170, -9.964067780447548373 ) ) ;
#21828 = CIRCLE ( 'NONE', #21032, 4.000000000000000000 ) ;
#21829 = CARTESIAN_POINT ( 'NONE',  ( 0.000000000000000000, 8.900000000000000355, 0.000000000000000000 ) ) ;
#21830 = CARTESIAN_POINT ( 'NONE',  ( 19.72076563415999928, 4.999595931465999676, -10.00405158629999924 ) ) ;
#21831 = CARTESIAN_POINT ( 'NONE',  ( -0.3358725919101999691, 28.67024443956999846, 2.064953224512999785 ) ) ;
#21832 = CARTESIAN_POINT ( 'NONE',  ( 13.60227460879853112, 6.956803079665641931, -5.741568056601168202 ) ) ;
#21833 = CARTESIAN_POINT ( 'NONE',  ( -4.754932747674998517, 12.62052246796000965, -0.7944665464532989496 ) ) ;
#21834 = CARTESIAN_POINT ( 'NONE',  ( -7.500000000000000000, 19.50000000000000000, -5.000000000000000000 ) ) ;
#21835 = ADVANCED_FACE ( 'NONE', ( #1352 ), #8743, .F. ) ;
#21836 = ORIENTED_EDGE ( 'NONE', *, *, #195, .T. ) ;
#21837 = AXIS2_PLACEMENT_3D ( 'NONE', #17616, #19679, #1145 ) ;
#21838 = DIRECTION ( 'NONE',  ( 0.000000000000000000, 0.000000000000000000, -1.000000000000000000 ) ) ;
#21839 = CARTESIAN_POINT ( 'NONE',  ( -2.500000000000000000, 29.03419673619000108, 0.000000000000000000 ) ) ;
#21840 = ORIENTED_EDGE ( 'NONE', *, *, #15327, .T. ) ;
#21841 = CARTESIAN_POINT ( 'NONE',  ( 11.66614181938224704, -12.78577920080955899, -2.854240613922053083 ) ) ;
#21842 = DIRECTION ( 'NONE',  ( 0.000000000000000000, 1.000000000000000000, 0.000000000000000000 ) ) ;
#21843 = CIRCLE ( 'NONE', #9851, 10.59999999999999964 ) ;
#21844 = CARTESIAN_POINT ( 'NONE',  ( 16.13671907226000002, 6.387739664468999656, -9.029444740878000530 ) ) ;
#21845 = ORIENTED_EDGE ( 'NONE', *, *, #20089, .T. ) ;
#21846 = B_SPLINE_CURVE_WITH_KNOTS ( 'NONE', 3,
 ( #15507, #21089, #8259, #21218 ),
 .UNSPECIFIED., .F., .F.,
 ( 4, 4 ),
 ( 0.000000000000000000, 1.000000000000000000 ),
 .UNSPECIFIED. ) ;
#21847 = CARTESIAN_POINT ( 'NONE',  ( -9.996213638770001353, -8.329006823806000881, 12.73688500997000084 ) ) ;
#21848 = CARTESIAN_POINT ( 'NONE',  ( 13.50000000000000000, 2.048741218006000064, 10.08990150394999930 ) ) ;
#21849 = FACE_BOUND ( 'NONE', #19436, .T. ) ;
#21850 = EDGE_CURVE ( 'NONE', #1329, #5868, #20386, .T. ) ;
#21851 = ORIENTED_EDGE ( 'NONE', *, *, #4997, .T. ) ;
#21852 = ADVANCED_FACE ( 'NONE', ( #3297 ), #19216, .T. ) ;
#21853 = CARTESIAN_POINT ( 'NONE',  ( 20.82328275621039282, -6.980445704735060986, 7.888708581122024555 ) ) ;
#21854 = CARTESIAN_POINT ( 'NONE',  ( -13.99999999999999822, 5.300363432082431103, 7.769144702572521766 ) ) ;
#21855 = CARTESIAN_POINT ( 'NONE',  ( 16.02407758412532601, -7.929595264181977576, -6.665930917639996345 ) ) ;
#21856 = CARTESIAN_POINT ( 'NONE',  ( -16.64019944616000046, 7.976360620752999786, -7.666729674259999960 ) ) ;
#21857 = CARTESIAN_POINT ( 'NONE',  ( -14.45960639177118701, -12.05326364612463408, 4.123067891182932598 ) ) ;
#21858 = AXIS2_PLACEMENT_3D ( 'NONE', #5583, #20135, #9691 ) ;
#21859 = CARTESIAN_POINT ( 'NONE',  ( -13.72667946694999941, 4.336095440212999641, 8.658528082053999597 ) ) ;
#21860 = CARTESIAN_POINT ( 'NONE',  ( 0.7926161359157861686, 29.95607633739005138, -2.009593667427580943 ) ) ;
#21861 = ADVANCED_FACE ( 'NONE', ( #23257, #6671 ), #12385, .F. ) ;
#21862 = ORIENTED_EDGE ( 'NONE', *, *, #2289, .F. ) ;
#21863 = CARTESIAN_POINT ( 'NONE',  ( 23.51329488828995551, -5.702615401652804117, 7.418699527094694268 ) ) ;
#21864 = ADVANCED_FACE ( 'NONE', ( #1701 ), #2981, .F. ) ;
#21865 = CARTESIAN_POINT ( 'NONE',  ( 19.41967423818407923, -10.43171934178962879, 1.169883962161388569 ) ) ;
#21866 = CARTESIAN_POINT ( 'NONE',  ( -0.8696119214085413773, 23.63534625394520461, -1.950261407548883552 ) ) ;
#21867 = ORIENTED_EDGE ( 'NONE', *, *, #4667, .T. ) ;
#21868 = CARTESIAN_POINT ( 'NONE',  ( 24.36165043081784276, -9.237917109185875830, -8.999458210778742639 ) ) ;
#21869 = CARTESIAN_POINT ( 'NONE',  ( -12.25000000000000000, 13.75000000000000000, 0.000000000000000000 ) ) ;
#21870 = CARTESIAN_POINT ( 'NONE',  ( -2.168383903499000898, 11.64268071799000559, -4.342811940312000019 ) ) ;
#21871 = EDGE_LOOP ( 'NONE', ( #10215, #3887, #7478, #20972, #23723 ) ) ;
#21872 = LINE ( 'NONE', #1645, #6875 ) ;
#21873 = ORIENTED_EDGE ( 'NONE', *, *, #16152, .F. ) ;
#21874 = AXIS2_PLACEMENT_3D ( 'NONE', #2673, #6179, #19512 ) ;
#21875 = DIRECTION ( 'NONE',  ( 1.000000000000000000, 0.000000000000000000, 0.000000000000000000 ) ) ;
#21876 = ITEM_DEFINED_TRANSFORMATION ( 'NONE', 'NONE', #10964,  #4390 ) ;
#21877 = DIRECTION ( 'NONE',  ( 1.000000000000000000, 0.000000000000000000, 0.000000000000000000 ) ) ;
#21878 = VERTEX_POINT ( 'NONE', #13071 ) ;
#21879 = CARTESIAN_POINT ( 'NONE',  ( -15.19472087121333637, -7.246037513405295449, 5.568446011427537812 ) ) ;
#21880 = CARTESIAN_POINT ( 'NONE',  ( -21.70673924429999957, -9.986630310228999718, -1.660063458803999970 ) ) ;
#21881 = DIRECTION ( 'NONE',  ( 0.8947368421052591669, 0.000000000000000000, 0.4465937565388801156 ) ) ;
#21882 = CARTESIAN_POINT ( 'NONE',  ( 19.05504166666666066, 7.325075730494997828, -5.629504654586422241 ) ) ;
#21883 = CARTESIAN_POINT ( 'NONE',  ( -23.98429299575930074, 10.59045595307713228, 0.3598248026102631725 ) ) ;
#21884 = CARTESIAN_POINT ( 'NONE',  ( -2.156038708526037517, 26.98917566598937867, -0.2605989890222873417 ) ) ;
#21885 = CARTESIAN_POINT ( 'NONE',  ( -5.330039164744003521, 15.50911245456000032, 2.864231857536000625 ) ) ;
#21886 = AXIS2_PLACEMENT_3D ( 'NONE', #5494, #18687, #16507 ) ;
#21887 = FACE_OUTER_BOUND ( 'NONE', #23785, .T. ) ;
#21888 = ORIENTED_EDGE ( 'NONE', *, *, #23015, .F. ) ;
#21889 = DIRECTION ( 'NONE',  ( 1.000000000000000000, 0.000000000000000000, 0.000000000000000000 ) ) ;
#21890 = CARTESIAN_POINT ( 'NONE',  ( 4.829988586904999437, 14.79876397742000016, 3.766541904039999888 ) ) ;
#21891 = CARTESIAN_POINT ( 'NONE',  ( 1.672490300650320449, 24.75097662330977144, 1.349479665860685351 ) ) ;
#21892 = VECTOR ( 'NONE', #5078, 1000.000000000000000 ) ;
#21893 = CARTESIAN_POINT ( 'NONE',  ( 2.256729627096000002, 27.96614211382000192, 0.4030006639746999686 ) ) ;
#21894 = B_SPLINE_CURVE_WITH_KNOTS ( 'NONE', 3,
 ( #4878, #12266, #3068, #23748, #8987, #6926, #7151, #3538 ),
 .UNSPECIFIED., .F., .F.,
 ( 4, 2, 2, 4 ),
 ( 0.000000000000000000, 0.2499999999999998890, 0.4999999999999997780, 1.000000000000000000 ),
 .UNSPECIFIED. ) ;
#21895 = CARTESIAN_POINT ( 'NONE',  ( 1.772600511826058822, 11.61607745207374975, 4.480042189610983883 ) ) ;
#21896 = EDGE_LOOP ( 'NONE', ( #156, #7778, #2720, #17950, #8107 ) ) ;
#21897 = ORIENTED_CLOSED_SHELL ( 'NONE', *, #5759, .F. );
#21898 = CARTESIAN_POINT ( 'NONE',  ( -1.981777970230752084, 11.64981023145996453, -4.391405225778299837 ) ) ;
#21899 = CARTESIAN_POINT ( 'NONE',  ( 2.329590180150573175, 27.99999999999984013, 3.273812635905912316 ) ) ;
#21900 = CARTESIAN_POINT ( 'NONE',  ( -1.997969690258423858, 30.09406483207807526, 1.094238623052827819 ) ) ;
#21901 = EDGE_LOOP ( 'NONE', ( #1562, #22499, #9848 ) ) ;
#21902 = DIRECTION ( 'NONE',  ( 1.000000000000000000, 0.000000000000000000, 0.000000000000000000 ) ) ;
#21903 = DIRECTION ( 'NONE',  ( -0.5000000000000169864, 0.000000000000000000, 0.8660254037844289376 ) ) ;
#21904 = AXIS2_PLACEMENT_3D ( 'NONE', #17348, #2704, #10206 ) ;
#21905 = CARTESIAN_POINT ( 'NONE',  ( 16.35468892131000018, 6.000265896171000257, 7.637201470843999473 ) ) ;
#21906 = CARTESIAN_POINT ( 'NONE',  ( 18.85894798992291399, 4.799130230538453112, 9.275998069617465092 ) ) ;
#21907 = DIRECTION ( 'NONE',  ( 0.000000000000000000, -1.000000000000000000, 0.000000000000000000 ) ) ;
#21908 = CARTESIAN_POINT ( 'NONE',  ( -1.980830272035999817, 30.09274665651000191, -0.8378900331165000104 ) ) ;
#21909 = CARTESIAN_POINT ( 'NONE',  ( 17.29108580085999947, -6.112256495352999863, 9.625372826315000907 ) ) ;
#21910 = CARTESIAN_POINT ( 'NONE',  ( 13.49999999999999467, -6.881482076045544183, 7.468481572847831096 ) ) ;
#21911 = EDGE_LOOP ( 'NONE', ( #1644, #3468 ) ) ;
#21912 = FACE_BOUND ( 'NONE', #7374, .T. ) ;
#21913 = CARTESIAN_POINT ( 'NONE',  ( 24.46803514405999991, 6.544162614452000426, 8.648843365141001271 ) ) ;
#21914 = CARTESIAN_POINT ( 'NONE',  ( -24.46466276874232904, 5.021295921611101498, -9.004480667326742349 ) ) ;
#21915 = AXIS2_PLACEMENT_3D ( 'NONE', #8428, #1159, #19328 ) ;
#21916 = CARTESIAN_POINT ( 'NONE',  ( 24.50000000000000000, -8.246372141814999779, 6.625187740483999832 ) ) ;
#21917 = CARTESIAN_POINT ( 'NONE',  ( -3.862330210613311721, 14.00496637028538593, 4.847486289291174977 ) ) ;
#21918 = CARTESIAN_POINT ( 'NONE',  ( -4.911810085394003877, 12.43822141189999542, -0.1532012021291000170 ) ) ;
#21919 = CARTESIAN_POINT ( 'NONE',  ( -23.81451776991000102, 9.879857505359000314, -5.177521040838999333 ) ) ;
#21920 = ORIENTED_EDGE ( 'NONE', *, *, #6829, .F. ) ;
#21921 = DIRECTION ( 'NONE',  ( 1.000000000000000000, 0.000000000000000000, 0.000000000000000000 ) ) ;
#21922 = CIRCLE ( 'NONE', #18061, 3.000000000000000000 ) ;
#21923 = CARTESIAN_POINT ( 'NONE',  ( 1.717816858030654537, 12.95705652094089366, 1.058607149792009094 ) ) ;
#21924 = ORIENTED_EDGE ( 'NONE', *, *, #1695, .F. ) ;
#21925 = ADVANCED_FACE ( 'NONE', ( #5458 ), #7261, .F. ) ;
#21926 = CARTESIAN_POINT ( 'NONE',  ( 0.3414794497234999726, 24.32349665651000237, -2.134113711687000148 ) ) ;
#21927 = CARTESIAN_POINT ( 'NONE',  ( 5.057845774443002540, 14.83209949158001884, 3.474588151562001404 ) ) ;
#21928 = CARTESIAN_POINT ( 'NONE',  ( 4.155001577763409948, 13.38046536914801266, 5.412598244128762559 ) ) ;
#21929 = DIRECTION ( 'NONE',  ( 0.000000000000000000, 0.000000000000000000, -1.000000000000000000 ) ) ;
#21930 = CARTESIAN_POINT ( 'NONE',  ( 1.536366799937286087, 27.71666666666666501, -1.999167105995451665 ) ) ;
#21931 = ORIENTED_EDGE ( 'NONE', *, *, #16453, .T. ) ;
#21932 = CARTESIAN_POINT ( 'NONE',  ( -17.78928642635000301, 9.027876325972000515, -3.804579355723999967 ) ) ;
#21933 = CARTESIAN_POINT ( 'NONE',  ( -7.834000000000000519, 1.320585629393000037E-14, 0.000000000000000000 ) ) ;
#21934 = AXIS2_PLACEMENT_3D ( 'NONE', #3422, #10803, #18196 ) ;
#21935 = DIRECTION ( 'NONE',  ( 1.000000000000000000, 0.000000000000000000, 0.000000000000000000 ) ) ;
#21936 = ORIENTED_EDGE ( 'NONE', *, *, #22523, .T. ) ;
#21937 = EDGE_CURVE ( 'NONE', #4988, #3964, #1938, .T. ) ;
#21938 = CARTESIAN_POINT ( 'NONE',  ( -10.88471959503360331, 15.34845819752904461, -1.727494947682089999 ) ) ;
#21939 = AXIS2_PLACEMENT_3D ( 'NONE', #519, #9618, #17002 ) ;
#21940 = CARTESIAN_POINT ( 'NONE',  ( -1.450143669890000098, 24.38504474195000071, -1.580009328412999903 ) ) ;
#21941 = CARTESIAN_POINT ( 'NONE',  ( 14.63547441700031548, 5.828595367498566659, -8.523805803212322729 ) ) ;
#21942 = PLANE ( 'NONE',  #22977 ) ;
#21943 = CARTESIAN_POINT ( 'NONE',  ( 24.05204201319999768, 10.75388736322999961, 3.479171898811000307 ) ) ;
#21944 = CARTESIAN_POINT ( 'NONE',  ( 0.6146774451941000583, 30.55152231057000023, -2.279116712825999702 ) ) ;
#21945 = CARTESIAN_POINT ( 'NONE',  ( 14.07248325032791314, 5.273353179838896843, 7.334521014497600078 ) ) ;
#21946 = CARTESIAN_POINT ( 'NONE',  ( -12.00000000000000000, 1.371604415045000054E-14, 0.000000000000000000 ) ) ;
#21947 = CARTESIAN_POINT ( 'NONE',  ( 4.749999884653000493, 15.09999988465641074, -5.093549567505999500E-08 ) ) ;
#21948 = ORIENTED_EDGE ( 'NONE', *, *, #13652, .T. ) ;
#21949 = CARTESIAN_POINT ( 'NONE',  ( -14.95696059356579433, -8.969510928318662479, -1.518716752286801031 ) ) ;
#21950 = LINE ( 'NONE', #21839, #23525 ) ;
#21951 = VECTOR ( 'NONE', #7143, 1000.000000000000000 ) ;
#21952 = ORIENTED_EDGE ( 'NONE', *, *, #13333, .T. ) ;
#21953 = EDGE_CURVE ( 'NONE', #23163, #17341, #12841, .T. ) ;
#21954 = CARTESIAN_POINT ( 'NONE',  ( -2.408749103101126554, 30.34919033230260865, -1.018899445479910071 ) ) ;
#21955 = CARTESIAN_POINT ( 'NONE',  ( 11.18529249867709474, -9.951874339551746829, -7.762889674110271976 ) ) ;
#21956 = AXIS2_PLACEMENT_3D ( 'NONE', #17279, #21030, #22839 ) ;
#21957 = CARTESIAN_POINT ( 'NONE',  ( 21.75799770046333137, 1.208283319978225689, 9.229634816791103091 ) ) ;
#21958 = CARTESIAN_POINT ( 'NONE',  ( 18.48258074425000075, 7.027092927644000397, 8.624643700690000969 ) ) ;
#21959 = CARTESIAN_POINT ( 'NONE',  ( -14.19545626576198138, -2.703128947221847156, 9.988535580370172084 ) ) ;
#21960 = ORIENTED_EDGE ( 'NONE', *, *, #20208, .F. ) ;
#21961 = CARTESIAN_POINT ( 'NONE',  ( -12.04003756584999962, 8.646183865892000497, -12.09541814886999944 ) ) ;
#21962 = DIRECTION ( 'NONE',  ( -1.000000000000000000, 0.000000000000000000, 0.000000000000000000 ) ) ;
#21963 = CARTESIAN_POINT ( 'NONE',  ( -14.43045961913871089, -12.44097983993757595, -3.451577511306503698 ) ) ;
#21964 = VERTEX_POINT ( 'NONE', #14882 ) ;
#21965 = EDGE_CURVE ( 'NONE', #9936, #3685, #12663, .T. ) ;
#21966 = CARTESIAN_POINT ( 'NONE',  ( 20.41147854889662838, 6.791870828880062660, 8.042442484653800960 ) ) ;
#21967 = CARTESIAN_POINT ( 'NONE',  ( 22.83443279375291368, 36.19190089707605296, 6.000000000000000000 ) ) ;
#21968 = CARTESIAN_POINT ( 'NONE',  ( 16.10246075293501633, -5.923530797957349492, -8.502184744949477846 ) ) ;
#21969 = AXIS2_PLACEMENT_3D ( 'NONE', #14123, #20059, #12317 ) ;
#21970 = B_SPLINE_CURVE_WITH_KNOTS ( 'NONE', 3,
 ( #19193, #10117, #21136, #17506, #22938, #3107, #23187, #4548, #16027, #19570, #13865, #2856, #900, #2974, #1025, #4795, #17993, #15551, #12179, #4915, #2735, #6355, #13987, #10365, #15666, #1158, #23421, #21378, #12062, #10239, #19692, #8302, #15796, #17754, #8551, #10491, #12302, #6481, #14232, #23056 ),
 .UNSPECIFIED., .F., .F.,
 ( 4, 2, 2, 1, 1, 2, 2, 2, 2, 2, 2, 2, 2, 1, 2, 2, 2, 2, 1, 2, 2, 4 ),
 ( 0.000000000000000000, 0.1250000000000027478, 0.1875000000000036637, 0.2187500000000025258, 0.2343750000000018319, 0.2421875000000017764, 0.2500000000000017208, 0.3125000000000177081, 0.3437500000000245359, 0.3593750000000291989, 0.3750000000000339173, 0.4375000000000564548, 0.4687500000000697775, 0.4843750000000763833, 0.4921875000000776601, 0.5000000000000789369, 0.6250000000000606182, 0.6875000000000502931, 0.7187500000000442979, 0.7343750000000424105, 0.7500000000000406342, 1.000000000000000000 ),
 .UNSPECIFIED. ) ;
#21971 = CARTESIAN_POINT ( 'NONE',  ( -18.94199577250666167, 4.611708388952700410, 8.001634414202589696 ) ) ;
#21972 = CARTESIAN_POINT ( 'NONE',  ( 2.095803007753000102, 29.79556831668999806, 0.6294804420801000111 ) ) ;
#21973 = CARTESIAN_POINT ( 'NONE',  ( -16.57050433853000015, -7.584645295112999897, -6.147042915735999813 ) ) ;
#21974 = EDGE_CURVE ( 'NONE', #6021, #21466, #11099, .T. ) ;
#21975 = AXIS2_PLACEMENT_3D ( 'NONE', #4765, #8025, #20137 ) ;
#21976 = CARTESIAN_POINT ( 'NONE',  ( 0.3068592026817785201, 29.98565460010522443, -2.141133321009449642 ) ) ;
#21977 = EDGE_LOOP ( 'NONE', ( #14818, #23688, #8677, #4826, #9232 ) ) ;
#21978 = CARTESIAN_POINT ( 'NONE',  ( -0.5691252486112998721, 23.64706705728999836, -2.185498830599999831 ) ) ;
#21979 = CARTESIAN_POINT ( 'NONE',  ( 20.10063544609122843, 6.579109543901849655, -8.200420943266742313 ) ) ;
#21980 = DIRECTION ( 'NONE',  ( 1.000000000000000000, 0.000000000000000000, 0.000000000000000000 ) ) ;
#21981 = ORIENTED_EDGE ( 'NONE', *, *, #5128, .T. ) ;
#21982 = EDGE_CURVE ( 'NONE', #21630, #3210, #19615, .T. ) ;
#21983 = CARTESIAN_POINT ( 'NONE',  ( 24.45564077607145492, -9.795255522623715905, -8.034119761694611839 ) ) ;
#21984 = CARTESIAN_POINT ( 'NONE',  ( -14.25243324638999809, -7.716878364870000340, -11.63397459621999985 ) ) ;
#21985 = EDGE_CURVE ( 'NONE', #8412, #17309, #10730, .T. ) ;
#21986 = CIRCLE ( 'NONE', #21206, 4.750000000000000000 ) ;
#21987 = CARTESIAN_POINT ( 'NONE',  ( 4.838659373281001486, 12.42377767764999419, -0.1101032568685000185 ) ) ;
#21988 = VERTEX_POINT ( 'NONE', #3640 ) ;
#21989 = DIRECTION ( 'NONE',  ( -0.000000000000000000, -1.000000000000000000, -0.000000000000000000 ) ) ;
#21990 = ORIENTED_EDGE ( 'NONE', *, *, #20755, .F. ) ;
#21991 = FACE_OUTER_BOUND ( 'NONE', #1483, .T. ) ;
#21992 = CARTESIAN_POINT ( 'NONE',  ( -4.749999884653000493, 15.09999988465641074, 5.093549627072000020E-08 ) ) ;
#21993 = VERTEX_POINT ( 'NONE', #5685 ) ;
#21994 = EDGE_CURVE ( 'NONE', #5259, #12884, #11331, .T. ) ;
#21995 = CARTESIAN_POINT ( 'NONE',  ( 22.85395603379666341, 4.662265998550135571, -8.089352615493318410 ) ) ;
#21996 = EDGE_CURVE ( 'NONE', #13227, #9372, #3388, .T. ) ;
#21997 = VECTOR ( 'NONE', #8335, 1000.000000000000000 ) ;
#21998 = CARTESIAN_POINT ( 'NONE',  ( -22.83084603907999721, 8.452768372852000667, -5.626295165922000407 ) ) ;
#21999 = CARTESIAN_POINT ( 'NONE',  ( -20.43329236144000305, -6.491487173960999613, 6.361872185110000189 ) ) ;
#22000 = CARTESIAN_POINT ( 'NONE',  ( -4.850028262036998328, 13.70733162851999865, -4.729463290261002761 ) ) ;
#22001 = CARTESIAN_POINT ( 'NONE',  ( -23.13503384608747027, -10.42901907143014739, 1.748523312326609513 ) ) ;
#22002 = CARTESIAN_POINT ( 'NONE',  ( 2.139890459600042316, 27.42644467189214907, -0.3715313211230960588 ) ) ;
#22003 = AXIS2_PLACEMENT_3D ( 'NONE', #13183, #18642, #14990 ) ;
#22004 = DIRECTION ( 'NONE',  ( -1.000000000000000000, 0.000000000000000000, 0.000000000000000000 ) ) ;
#22005 = CARTESIAN_POINT ( 'NONE',  ( -0.9744765624120647063, 29.91693820796410463, 4.056187847889995091 ) ) ;
#22006 = VERTEX_POINT ( 'NONE', #14763 ) ;
#22007 = CARTESIAN_POINT ( 'NONE',  ( -17.23547087121333732, -1.193091500503335789, 9.113577864919761851 ) ) ;
#22008 = CARTESIAN_POINT ( 'NONE',  ( 3.952348409963450049, 14.44207180802359147, 4.679171297609252989 ) ) ;
#22009 = CARTESIAN_POINT ( 'NONE',  ( 1.248966013227574168, 24.78517284287330114, 1.711384895940772699 ) ) ;
#22010 = AXIS2_PLACEMENT_3D ( 'NONE', #9249, #2209, #22989 ) ;
#22011 = DIRECTION ( 'NONE',  ( 0.000000000000000000, -1.000000000000000000, 0.000000000000000000 ) ) ;
#22012 = CARTESIAN_POINT ( 'NONE',  ( -1.996229403933999835, 28.69771896306000158, 1.117936111508999852 ) ) ;
#22013 = CIRCLE ( 'NONE', #14659, 0.5000000000000004441 ) ;
#22014 = CARTESIAN_POINT ( 'NONE',  ( 1.268068893756492344, 11.54954083627711192, 4.648988597672141232 ) ) ;
#22015 = VERTEX_POINT ( 'NONE', #3532 ) ;
#22016 = CARTESIAN_POINT ( 'NONE',  ( -3.428826227638388957, 11.97595429753372009, -3.402799634008572660 ) ) ;
#22017 = CARTESIAN_POINT ( 'NONE',  ( -10.51102833032320483, 15.52504438449052060, 1.381747433397627178 ) ) ;
#22018 = CIRCLE ( 'NONE', #20464, 15.43375672974000068 ) ;
#22019 = PLANE ( 'NONE',  #5674 ) ;
#22020 = ORIENTED_EDGE ( 'NONE', *, *, #3228, .T. ) ;
#22021 = EDGE_CURVE ( 'NONE', #19135, #14395, #2202, .T. ) ;
#22022 = DIRECTION ( 'NONE',  ( 0.000000000000000000, -1.000000000000000000, 0.000000000000000000 ) ) ;
#22023 = CARTESIAN_POINT ( 'NONE',  ( -16.44184587121332441, -2.380011688135305281, -8.856588498222468075 ) ) ;
#22024 = CARTESIAN_POINT ( 'NONE',  ( 11.85750142130999940, -4.891210171397999851, -8.253706317253998392 ) ) ;
#22025 = CARTESIAN_POINT ( 'NONE',  ( 18.58429248281415624, 10.33569022815195027, 1.375693033861695280 ) ) ;
#22026 = UNCERTAINTY_MEASURE_WITH_UNIT (LENGTH_MEASURE( 1.000000000000000082E-05 ), #6673, 'distance_accuracy_value', 'NONE');
#22027 = CIRCLE ( 'NONE', #11587, 2.673746900119611247 ) ;
#22028 = CARTESIAN_POINT ( 'NONE',  ( -24.46742986863897329, 1.281690452090803456, 12.50000620969185938 ) ) ;
#22029 = CARTESIAN_POINT ( 'NONE',  ( 1.846653654530999944, 29.93346240518999934, -1.440075676530000015 ) ) ;
#22030 = CARTESIAN_POINT ( 'NONE',  ( -12.49274363707000113, 6.877373328682999443, -5.798644816960000448 ) ) ;
#22031 = CARTESIAN_POINT ( 'NONE',  ( 13.50000000000000000, -9.115747871093871524, 3.863369538079849619 ) ) ;
#22032 = AXIS2_PLACEMENT_3D ( 'NONE', #3833, #23932, #7340 ) ;
#22033 = EDGE_LOOP ( 'NONE', ( #17278, #3725, #5902, #15528 ) ) ;
#22034 = VECTOR ( 'NONE', #5669, 1000.000000000000227 ) ;
#22035 = CARTESIAN_POINT ( 'NONE',  ( -24.47970833437436156, 11.33727345181091550, 5.363206565949876214 ) ) ;
#22036 = CARTESIAN_POINT ( 'NONE',  ( 19.77050301799999943, -3.010326857828999891, -10.83590067529000045 ) ) ;
#22037 = CARTESIAN_POINT ( 'NONE',  ( -24.15753426113404956, 8.341958059169604311, 5.501469373877088564 ) ) ;
#22038 = CARTESIAN_POINT ( 'NONE',  ( 1.600000000000000089, 9.000000000000000000, 0.000000000000000000 ) ) ;
#22039 = CARTESIAN_POINT ( 'NONE',  ( 4.724999999999999645, 13.10000000000000142, 0.000000000000000000 ) ) ;
#22040 = CARTESIAN_POINT ( 'NONE',  ( 4.698522026118003403, 12.42251073348998425, 1.557367633878998348 ) ) ;
#22041 = CARTESIAN_POINT ( 'NONE',  ( -1.127947703010715230, 29.27359719799922999, -1.846395287258788098 ) ) ;
#22042 = FACE_OUTER_BOUND ( 'NONE', #6970, .T. ) ;
#22043 = ORIENTED_EDGE ( 'NONE', *, *, #5972, .T. ) ;
#22044 = CARTESIAN_POINT ( 'NONE',  ( 2.394884942776999814, 23.89488494277999919, 0.000000000000000000 ) ) ;
#22045 = ORIENTED_EDGE ( 'NONE', *, *, #2462, .T. ) ;
#22046 = CARTESIAN_POINT ( 'NONE',  ( 2.053067944554000324, 24.18415609745999717, -0.6752492679973999268 ) ) ;
#22047 = CARTESIAN_POINT ( 'NONE',  ( 6.112958255465001045, 13.74060334821000318, 1.425172817424000149 ) ) ;
#22048 = CARTESIAN_POINT ( 'NONE',  ( 11.12576011241567109, -1.246535810014351764, -12.50000754954019833 ) ) ;
#22049 = CARTESIAN_POINT ( 'NONE',  ( -4.624999999996013855, 15.00000000000000000, 0.000000000000000000 ) ) ;
#22050 = DIRECTION ( 'NONE',  ( 1.000000000000000000, 0.000000000000000000, 0.000000000000000000 ) ) ;
#22051 = CARTESIAN_POINT ( 'NONE',  ( 18.27225174930999785, 9.757448129154999705, -4.584997352848999341 ) ) ;
#22052 =( LENGTH_UNIT ( ) NAMED_UNIT ( * ) SI_UNIT ( .MILLI., .METRE. ) );
#22053 = ORIENTED_EDGE ( 'NONE', *, *, #13234, .T. ) ;
#22054 = CARTESIAN_POINT ( 'NONE',  ( -18.19554712229000160, -2.285746783449999597, -9.537972663088998715 ) ) ;
#22055 = DIRECTION ( 'NONE',  ( 0.000000000000000000, 1.000000000000000000, 0.000000000000000000 ) ) ;
#22056 = CARTESIAN_POINT ( 'NONE',  ( 10.35615758860000035, 0.000000000000000000, 0.000000000000000000 ) ) ;
#22057 = VERTEX_POINT ( 'NONE', #22049 ) ;
#22058 = CARTESIAN_POINT ( 'NONE',  ( -20.67707759490999919, -0.1471764284891000085, -11.21320839060999930 ) ) ;
#22059 = CARTESIAN_POINT ( 'NONE',  ( -1.802411599998000158, 25.21757922916000183, -1.162178362301999890 ) ) ;
#22060 = CARTESIAN_POINT ( 'NONE',  ( 14.65172699290454972, 6.282441235618426489, -8.192983905010713386 ) ) ;
#22061 = DIRECTION ( 'NONE',  ( 1.000000000000000000, 0.000000000000000000, 0.000000000000000000 ) ) ;
#22062 = CARTESIAN_POINT ( 'NONE',  ( 24.78622986507000192, -10.15669625742000015, 2.982069395447000115 ) ) ;
#22063 = EDGE_CURVE ( 'NONE', #18634, #4798, #15942, .T. ) ;
#22064 = CARTESIAN_POINT ( 'NONE',  ( 1.344136286029000038, 29.00535257235999964, -1.701023518473999907 ) ) ;
#22065 = CARTESIAN_POINT ( 'NONE',  ( 14.09167841898807438, 4.781097061663486691, 7.663137420670809163 ) ) ;
#22066 = CARTESIAN_POINT ( 'NONE',  ( 1.385371806688001639, 11.73739883782001314, -4.651319360739003095 ) ) ;
#22067 = DIRECTION ( 'NONE',  ( 0.000000000000000000, -1.000000000000000000, 0.000000000000000000 ) ) ;
#22068 = VERTEX_POINT ( 'NONE', #7220 ) ;
#22069 = CARTESIAN_POINT ( 'NONE',  ( -14.67092228382045782, -3.603863581076387490, -8.324530791617933190 ) ) ;
#22070 = DIRECTION ( 'NONE',  ( -1.000000000000000000, 0.000000000000000000, 0.000000000000000000 ) ) ;
#22071 = VERTEX_POINT ( 'NONE', #19958 ) ;
#22072 = DIRECTION ( 'NONE',  ( 1.000000000000000000, 0.000000000000000000, 0.000000000000000000 ) ) ;
#22073 = CARTESIAN_POINT ( 'NONE',  ( 11.36448692219090084, -9.446283672508670293, -8.638507912415571255 ) ) ;
#22074 = EDGE_CURVE ( 'NONE', #12394, #4710, #16506, .T. ) ;
#22075 = CARTESIAN_POINT ( 'NONE',  ( -10.35615758860000035, -7.000000000000000000, 0.000000000000000000 ) ) ;
#22076 = CARTESIAN_POINT ( 'NONE',  ( 13.42244730194000013, 3.896089010268000141, 9.766325367788999401 ) ) ;
#22077 = CARTESIAN_POINT ( 'NONE',  ( -16.37253276963559756, 8.717735455328519123, 5.679932193535492502 ) ) ;
#22078 = CARTESIAN_POINT ( 'NONE',  ( -2.665093312283999705, 26.68712896666999868, 0.1571687770952999719 ) ) ;
#22079 = EDGE_LOOP ( 'NONE', ( #12323, #4013, #17102, #11972, #10200, #8562 ) ) ;
#22080 = CARTESIAN_POINT ( 'NONE',  ( -9.283456138769999200, 6.248931676845000283, -13.87633134369000132 ) ) ;
#22081 = CARTESIAN_POINT ( 'NONE',  ( 13.49999999999999289, 9.584200888098308724, 0.3179355005750706953 ) ) ;
#22082 = CARTESIAN_POINT ( 'NONE',  ( -14.37382028566586101, -13.01774735371480318, -2.452106660102837843 ) ) ;
#22083 = ORIENTED_EDGE ( 'NONE', *, *, #18884, .T. ) ;
#22084 = CARTESIAN_POINT ( 'NONE',  ( 23.05879131019755235, -8.652720740703848890, -6.105659068090134589 ) ) ;
#22085 = CARTESIAN_POINT ( 'NONE',  ( 24.37173283531060619, 9.297778257491829734, -8.895775660514537719 ) ) ;
#22086 = CARTESIAN_POINT ( 'NONE',  ( 16.16828646285382476, -3.839896425325243889, -9.652464845986353126 ) ) ;
#22087 = CARTESIAN_POINT ( 'NONE',  ( -15.88350446789000081, -7.863141422307999839, 7.753313641256998956 ) ) ;
#22088 = EDGE_CURVE ( 'NONE', #11775, #3633, #9555, .T. ) ;
#22089 = CARTESIAN_POINT ( 'NONE',  ( 0.3908479946973999475, 29.99303757602000076, -2.310142352749000150 ) ) ;
#22090 = CARTESIAN_POINT ( 'NONE',  ( -17.83004450757999848, 9.857337362280999216, 3.100493417357999881 ) ) ;
#22091 = CARTESIAN_POINT ( 'NONE',  ( 2.145295876472778751, 29.81890497885072833, -0.2554101685241636499 ) ) ;
#22092 = VERTEX_POINT ( 'NONE', #12804 ) ;
#22093 = CARTESIAN_POINT ( 'NONE',  ( -2.322746915978000093, 24.60096985244999956, -0.2454950339001999993 ) ) ;
#22094 = CARTESIAN_POINT ( 'NONE',  ( 21.32069094358849526, -10.50854990665072997, -1.992772991833056562 ) ) ;
#22095 = CARTESIAN_POINT ( 'NONE',  ( 0.000000000000000000, 19.00000000000000000, 0.000000000000000000 ) ) ;
#22096 = EDGE_LOOP ( 'NONE', ( #6486, #4746, #18220, #13479, #18567 ) ) ;
#22097 = CARTESIAN_POINT ( 'NONE',  ( 24.07420734439622123, -5.678657336859300742, 12.50000000000000355 ) ) ;
#22098 = CARTESIAN_POINT ( 'NONE',  ( 4.856921901366256122, 14.53926045619292751, -3.784552473569310571 ) ) ;
#22099 = EDGE_CURVE ( 'NONE', #20167, #9887, #13029, .T. ) ;
#22100 = CARTESIAN_POINT ( 'NONE',  ( -4.856048418805002598, 12.41684859253000361, -0.7982404537521002874 ) ) ;
#22101 = ORIENTED_EDGE ( 'NONE', *, *, #14737, .T. ) ;
#22102 = CARTESIAN_POINT ( 'NONE',  ( 14.13450125731000107, 8.592455601080001060, 3.130286720869000394 ) ) ;
#22103 = ORIENTED_EDGE ( 'NONE', *, *, #14723, .F. ) ;
#22104 = CARTESIAN_POINT ( 'NONE',  ( -4.972490738245377351, 15.85507734270906077, 3.578469026183233037 ) ) ;
#22105 = PRODUCT_CONTEXT ( 'NONE', #17953, 'mechanical' ) ;
#22106 = ADVANCED_FACE ( 'NONE', ( #3253 ), #5188, .F. ) ;
#22107 = CARTESIAN_POINT ( 'NONE',  ( -7.034000000000000696, -11.50000000000000000, 0.000000000000000000 ) ) ;
#22108 = VERTEX_POINT ( 'NONE', #7106 ) ;
#22109 = CARTESIAN_POINT ( 'NONE',  ( -23.39536544476928981, -2.238522300281205801, -9.155022575166720245 ) ) ;
#22110 = APPLICATION_CONTEXT ( 'automotive_design' ) ;
#22111 = CARTESIAN_POINT ( 'NONE',  ( -25.18765372902999999, 0.3463529480658999460, -9.692089422165000911 ) ) ;
#22112 = EDGE_CURVE ( 'NONE', #11620, #2581, #19703, .T. ) ;
#22113 = CARTESIAN_POINT ( 'NONE',  ( 11.78693030655906782, -8.669062849295544382, -9.984739426234524373 ) ) ;
#22114 = CARTESIAN_POINT ( 'NONE',  ( -4.012811773491001155, 13.17015569023999610, -4.696507356432001679 ) ) ;
#22115 = EDGE_CURVE ( 'NONE', #2581, #4204, #36, .T. ) ;
#22116 = CARTESIAN_POINT ( 'NONE',  ( -24.44752525921816044, 0.002284610134966501369, -10.60947411550792729 ) ) ;
#22117 = CARTESIAN_POINT ( 'NONE',  ( -1.549481145645184021, 27.90346540521953145, 1.523379885845690618 ) ) ;
#22118 = CARTESIAN_POINT ( 'NONE',  ( 16.33404166666666057, -7.269238015384150486, 5.586593178390435455 ) ) ;
#22119 = CARTESIAN_POINT ( 'NONE',  ( 1.687576972922000040, 28.34000240010000127, 2.322750540216000026 ) ) ;
#22120 = CARTESIAN_POINT ( 'NONE',  ( 1.766725490425707035, 30.68186832659927532, -1.242484399774119508 ) ) ;
#22121 = ORIENTED_EDGE ( 'NONE', *, *, #11448, .F. ) ;
#22122 = DIRECTION ( 'NONE',  ( 0.000000000000000000, -0.5000000000000169864, -0.8660254037844288266 ) ) ;
#22123 = DIRECTION ( 'NONE',  ( -1.351954405892998782E-08, -0.9999999999999990008, -4.357971222333990821E-08 ) ) ;
#22124 = CARTESIAN_POINT ( 'NONE',  ( -21.07269641591645026, -10.52253052917413001, -0.05638204554735719992 ) ) ;
#22125 = CARTESIAN_POINT ( 'NONE',  ( -1.195388535980999922, 28.50271896306000485, -1.950678319476999878 ) ) ;
#22126 = EDGE_CURVE ( 'NONE', #10277, #11958, #10485, .T. ) ;
#22127 = CARTESIAN_POINT ( 'NONE',  ( -2.130581439410940359, 30.85744147019555328, 0.2262312255918205728 ) ) ;
#22128 = FACE_OUTER_BOUND ( 'NONE', #16639, .T. ) ;
#22129 = ORIENTED_EDGE ( 'NONE', *, *, #15154, .T. ) ;
#22130 = CARTESIAN_POINT ( 'NONE',  ( -4.194936859874647261, 12.21355901615086559, -2.415068615545117758 ) ) ;
#22131 = CARTESIAN_POINT ( 'NONE',  ( -4.000000000000000000, 28.00000000000000000, 0.000000000000000000 ) ) ;
#22132 = CARTESIAN_POINT ( 'NONE',  ( 0.000000000000000000, 28.15000000000000213, 0.000000000000000000 ) ) ;
#22133 = ORIENTED_EDGE ( 'NONE', *, *, #10473, .T. ) ;
#22134 = CARTESIAN_POINT ( 'NONE',  ( 11.77156519342000074, 1.080486702797000030E-14, 0.000000000000000000 ) ) ;
#22135 = CARTESIAN_POINT ( 'NONE',  ( 18.46518908530999781, 4.839936825908999651, 9.065913725881001639 ) ) ;
#22136 = CARTESIAN_POINT ( 'NONE',  ( 18.58923523000861877, 10.30907166458805690, 1.558049498255399845 ) ) ;
#22137 = EDGE_CURVE ( 'NONE', #6064, #17452, #11025, .T. ) ;
#22138 = CARTESIAN_POINT ( 'NONE',  ( 0.000000000000000000, 24.50000000000000000, 0.000000000000000000 ) ) ;
#22139 = CARTESIAN_POINT ( 'NONE',  ( 2.214406098997000250, 29.00694631853999894, 0.7617925945809999044 ) ) ;
#22140 = ADVANCED_FACE ( 'NONE', ( #12184 ), #13056, .F. ) ;
#22141 = CARTESIAN_POINT ( 'NONE',  ( 18.30671080085999947, 9.244294984138999638, -6.722868547277000673 ) ) ;
#22142 = CARTESIAN_POINT ( 'NONE',  ( 13.49999999999999289, -8.867844327939206295, 4.500207874338363112 ) ) ;
#22143 = AXIS2_PLACEMENT_3D ( 'NONE', #18538, #20242, #13194 ) ;
#22144 = VERTEX_POINT ( 'NONE', #16126 ) ;
#22145 = CARTESIAN_POINT ( 'NONE',  ( -1.259047450927232026, 28.93333333333333712, 2.184465970885653974 ) ) ;
#22146 = CARTESIAN_POINT ( 'NONE',  ( 20.21885669234999838, 3.601023353282000183, -10.10703359440999982 ) ) ;
#22147 = CARTESIAN_POINT ( 'NONE',  ( -24.05515809193239818, 4.205914552781904625, 8.947780035611691218 ) ) ;
#22148 = ORIENTED_EDGE ( 'NONE', *, *, #22393, .F. ) ;
#22149 = CARTESIAN_POINT ( 'NONE',  ( 24.49999999999999645, -5.925652364458730226, 8.763099245663633852 ) ) ;
#22150 = CARTESIAN_POINT ( 'NONE',  ( 24.50000000000000355, 6.882980620445878550, 7.423222315167702590 ) ) ;
#22151 = CARTESIAN_POINT ( 'NONE',  ( 3.409885634504002283, 11.93905035093000677, 3.554569955099000200 ) ) ;
#22152 = CARTESIAN_POINT ( 'NONE',  ( 0.3047452333598806851, 29.18569219383820013, -2.138379523722714115 ) ) ;
#22153 = FACE_OUTER_BOUND ( 'NONE', #15949, .T. ) ;
#22154 = ORIENTED_EDGE ( 'NONE', *, *, #14309, .T. ) ;
#22155 = EDGE_CURVE ( 'NONE', #19900, #9967, #23461, .T. ) ;
#22156 = CARTESIAN_POINT ( 'NONE',  ( -1.767805011140364924, 26.50018596745192312, 1.767686163102024643 ) ) ;
#22157 = ORIENTED_EDGE ( 'NONE', *, *, #17985, .T. ) ;
#22158 = CARTESIAN_POINT ( 'NONE',  ( -2.193166068984999661, 23.80189877136000121, -0.8531035950795999856 ) ) ;
#22159 = CARTESIAN_POINT ( 'NONE',  ( 6.265492238153998805, 13.70414734520999112, 0.3873945776806000940 ) ) ;
#22160 = CARTESIAN_POINT ( 'NONE',  ( 11.85409292834066264, -4.507814091389457545, -12.50002426122858168 ) ) ;
#22161 = CARTESIAN_POINT ( 'NONE',  ( 19.05233531832000082, -1.887707665395999879, 10.26617185442000135 ) ) ;
#22162 = DIRECTION ( 'NONE',  ( -1.000000000000000000, 0.000000000000000000, 0.000000000000000000 ) ) ;
#22163 = CARTESIAN_POINT ( 'NONE',  ( 17.83350174931000254, -4.076359992019000344, -9.968186170592000295 ) ) ;
#22164 = EDGE_LOOP ( 'NONE', ( #10638, #19034, #19519, #9938 ) ) ;
#22165 = CARTESIAN_POINT ( 'NONE',  ( -17.38302573041000088, 5.218320932965999859, 8.277968099418000492 ) ) ;
#22166 = CARTESIAN_POINT ( 'NONE',  ( 0.000000000000000000, 31.00000000000000000, 0.000000000000000000 ) ) ;
#22167 = LINE ( 'NONE', #8748, #17098 ) ;
#22168 = ORIENTED_EDGE ( 'NONE', *, *, #4039, .T. ) ;
#22169 = CARTESIAN_POINT ( 'NONE',  ( -10.68259645647714429, 15.42389723940939739, -1.538719359861782099 ) ) ;
#22170 = CARTESIAN_POINT ( 'NONE',  ( 2.103662084068000038, 24.72789791218000133, 1.013534942017999985 ) ) ;
#22171 = CARTESIAN_POINT ( 'NONE',  ( 14.77189528956980347, 9.067954214462249141, -4.942123315334161049 ) ) ;
#22172 = DIRECTION ( 'NONE',  ( 0.000000000000000000, -1.000000000000000000, 0.000000000000000000 ) ) ;
#22173 = CARTESIAN_POINT ( 'NONE',  ( 22.91383486932000224, -6.129809015165000652, 9.458891919796998948 ) ) ;
#22174 = CARTESIAN_POINT ( 'NONE',  ( 0.3237282180201000448, 29.40258014098999695, 2.338245789995000212 ) ) ;
#22175 = CARTESIAN_POINT ( 'NONE',  ( 14.10179216132728719, 4.514300806135581823, 7.822680230860565409 ) ) ;
#22176 = CARTESIAN_POINT ( 'NONE',  ( -6.634681955164054123, 15.38524051851555363, -1.622884314630087754 ) ) ;
#22177 = CARTESIAN_POINT ( 'NONE',  ( -6.781029893680056375, 15.33022057605113631, 1.804325008919367201 ) ) ;
#22178 = CARTESIAN_POINT ( 'NONE',  ( 11.31235608930338721, 12.07787442524536026, -4.080443649690880470 ) ) ;
#22179 = ORIENTED_EDGE ( 'NONE', *, *, #16075, .T. ) ;
#22180 = CARTESIAN_POINT ( 'NONE',  ( -1.944991678923578826, 24.14582603393633775, -1.623355076449641388 ) ) ;
#22181 = DIRECTION ( 'NONE',  ( -1.000000000000000000, 0.000000000000000000, 0.000000000000000000 ) ) ;
#22182 = ORIENTED_EDGE ( 'NONE', *, *, #15163, .T. ) ;
#22183 = CARTESIAN_POINT ( 'NONE',  ( -8.099999999999999645, -10.59999999999999964, -4.735481798356999505E-10 ) ) ;
#22184 = CARTESIAN_POINT ( 'NONE',  ( 21.98474770046333049, -5.675527994026910328, 7.385375838905533286 ) ) ;
#22185 = CARTESIAN_POINT ( 'NONE',  ( 18.02019104568000429, -6.876349436605000420, -8.728898656365000619 ) ) ;
#22186 = CARTESIAN_POINT ( 'NONE',  ( -6.250000012226999857, 15.73199627394999922, 1.185103398761000015 ) ) ;
#22187 = ADVANCED_FACE ( 'NONE', ( #7058 ), #15770, .F. ) ;
#22188 = CARTESIAN_POINT ( 'NONE',  ( -0.6232602838478999985, 25.81756359724000305, -2.388357610153000188 ) ) ;
#22189 = ORIENTED_EDGE ( 'NONE', *, *, #6674, .F. ) ;
#22190 = CARTESIAN_POINT ( 'NONE',  ( -11.42910256584999829, -0.5664460622508999954, 14.85721958263000175 ) ) ;
#22191 = CARTESIAN_POINT ( 'NONE',  ( 0.8542036545951054993, 6.831035656885031671, -1.528947743710137308 ) ) ;
#22192 = AXIS2_PLACEMENT_3D ( 'NONE', #13499, #2734, #17505 ) ;
#22193 = DIRECTION ( 'NONE',  ( 0.000000000000000000, 1.000000000000000000, 0.000000000000000000 ) ) ;
#22194 = ORIENTED_EDGE ( 'NONE', *, *, #2067, .T. ) ;
#22195 = CARTESIAN_POINT ( 'NONE',  ( -24.33938584176032904, 9.417644943808182845, 8.688014043592605873 ) ) ;
#22196 = CARTESIAN_POINT ( 'NONE',  ( 19.49962637556187772, -6.917197816422240741, -7.905051631841183202 ) ) ;
#22197 = CARTESIAN_POINT ( 'NONE',  ( 24.40278699097224546, 9.495349905928280876, -8.553571527287482823 ) ) ;
#22198 = CARTESIAN_POINT ( 'NONE',  ( 15.92969900157650187, -9.688817912527115439, -3.663007575884178024 ) ) ;
#22199 = CARTESIAN_POINT ( 'NONE',  ( -19.10140242030999858, -4.547125262218999708, -10.15970676401999917 ) ) ;
#22200 = CARTESIAN_POINT ( 'NONE',  ( 1.545690893027000135, 28.68824721936999822, 1.555291323814000037 ) ) ;
#22201 = CARTESIAN_POINT ( 'NONE',  ( -16.40813207178999988, 5.092047131649000136, -8.946165747030999427 ) ) ;
#22202 = CARTESIAN_POINT ( 'NONE',  ( -0.05303640295588081532, 29.60074729647491409, 2.159234738230836559 ) ) ;
#22203 = ORIENTED_EDGE ( 'NONE', *, *, #23312, .T. ) ;
#22204 = CARTESIAN_POINT ( 'NONE',  ( -1.617171946415000061, 25.28260575739999894, 1.470668775339999845 ) ) ;
#22205 = CARTESIAN_POINT ( 'NONE',  ( 22.39887952277467420, 7.496365056892780210, 7.455554306885533222 ) ) ;
#22206 = CARTESIAN_POINT ( 'NONE',  ( -1.963703823225463774, 26.25920717875808563, 0.8995588027868727243 ) ) ;
#22207 = EDGE_LOOP ( 'NONE', ( #17868, #11726, #858, #20260 ) ) ;
#22208 = CARTESIAN_POINT ( 'NONE',  ( -5.147747017024999039, 14.44777671499001315, 4.022432192786999927 ) ) ;
#22209 = CARTESIAN_POINT ( 'NONE',  ( 17.92129166666665085, -1.195141376095407493, 9.131177378213125806 ) ) ;
#22210 = EDGE_CURVE ( 'NONE', #14425, #3901, #16498, .T. ) ;
#22211 = CARTESIAN_POINT ( 'NONE',  ( 14.24418875730999900, 6.821019272440999259, 6.095525253705999624 ) ) ;
#22212 = EDGE_LOOP ( 'NONE', ( #20686, #11618, #2049 ) ) ;
#22213 = CARTESIAN_POINT ( 'NONE',  ( -0.3272492347489122655, 28.41753006952333749, 2.500000000000003553 ) ) ;
#22214 = CARTESIAN_POINT ( 'NONE',  ( -14.45561360440065890, -2.584657965311079941, -12.49996445837131276 ) ) ;
#22215 = ORIENTED_EDGE ( 'NONE', *, *, #12790, .T. ) ;
#22216 = DIRECTION ( 'NONE',  ( -8.881784197001252323E-16, 0.000000000000000000, 1.000000000000000000 ) ) ;
#22217 = CARTESIAN_POINT ( 'NONE',  ( 4.222040842892996970, 12.42583961254000968, 2.326471633585998067 ) ) ;
#22218 = VECTOR ( 'NONE', #7906, 1000.000000000000000 ) ;
#22219 = EDGE_CURVE ( 'NONE', #10732, #19490, #8714, .T. ) ;
#22220 = CARTESIAN_POINT ( 'NONE',  ( 11.48696334737605085, -9.189637287600886495, -9.082924181340967351 ) ) ;
#22221 = CARTESIAN_POINT ( 'NONE',  ( 18.41258333333331620, -8.905845225604863913, -2.393249065827368405 ) ) ;
#22222 = DIRECTION ( 'NONE',  ( 0.000000000000000000, 0.000000000000000000, 1.000000000000000000 ) ) ;
#22223 = CARTESIAN_POINT ( 'NONE',  ( -23.74465998031000069, 13.93375672974000068, 0.8660254037843999608 ) ) ;
#22224 =( GEOMETRIC_REPRESENTATION_CONTEXT ( 3 ) GLOBAL_UNCERTAINTY_ASSIGNED_CONTEXT ( ( #23717 ) ) GLOBAL_UNIT_ASSIGNED_CONTEXT ( ( #1957, #19012, #595 ) ) REPRESENTATION_CONTEXT ( 'NONE', 'WORKASPACE' ) );
#22225 = DIRECTION ( 'NONE',  ( 0.7071067811864258923, 0.7071067811862259411, 7.917084081357289653E-07 ) ) ;
#22226 = DIRECTION ( 'NONE',  ( 0.5000000000000169864, -0.8660254037844288266, 0.000000000000000000 ) ) ;
#22227 = DIRECTION ( 'NONE',  ( 0.000000000000000000, 0.000000000000000000, 1.000000000000000000 ) ) ;
#22228 = ORIENTED_EDGE ( 'NONE', *, *, #6087, .F. ) ;
#22229 = CARTESIAN_POINT ( 'NONE',  ( 22.87997594487999820, 7.046585999850999649, -6.898543380703000771 ) ) ;
#22230 = CARTESIAN_POINT ( 'NONE',  ( 1.649278745378622180, 24.74235546451014400, 1.391239989081180406 ) ) ;
#22231 = CARTESIAN_POINT ( 'NONE',  ( -23.88421579307469855, 10.09359931140187783, -3.213991999759431728 ) ) ;
#22232 = CARTESIAN_POINT ( 'NONE',  ( 0.1346854910757999679, 27.62521896306000357, -2.283846754818999791 ) ) ;
#22233 = CONICAL_SURFACE ( 'NONE', #2931, 4.309401076758999416, 1.119376321708719590 ) ;
#22234 = CARTESIAN_POINT ( 'NONE',  ( 3.258516839496470752, 11.92856103705473636, 3.566823035891872440 ) ) ;
#22235 = EDGE_LOOP ( 'NONE', ( #23622, #13171, #9638, #16347, #13838, #17984 ) ) ;
#22236 = EDGE_CURVE ( 'NONE', #14845, #9831, #3082, .T. ) ;
#22237 = CARTESIAN_POINT ( 'NONE',  ( -4.794898800817616547, 12.42857861981699941, -0.8372831007215363330 ) ) ;
#22238 = CARTESIAN_POINT ( 'NONE',  ( -5.194121241777001075, -12.44999999999999929, 0.000000000000000000 ) ) ;
#22239 = DIRECTION ( 'NONE',  ( 0.000000000000000000, -1.000000000000000000, 0.000000000000000000 ) ) ;
#22240 = ORIENTED_EDGE ( 'NONE', *, *, #5417, .T. ) ;
#22241 = LINE ( 'NONE', #9419, #6082 ) ;
#22242 = CARTESIAN_POINT ( 'NONE',  ( 13.85831408531000086, -6.842896344163999167, -7.504413997217999288 ) ) ;
#22243 = CARTESIAN_POINT ( 'NONE',  ( 18.03882547314998774, -1.826631431717876675, -10.26437193003392245 ) ) ;
#22244 = EDGE_CURVE ( 'NONE', #3210, #20052, #10329, .T. ) ;
#22245 = DIRECTION ( 'NONE',  ( 0.000000000000000000, 1.000000000000000000, 0.000000000000000000 ) ) ;
#22246 = CARTESIAN_POINT ( 'NONE',  ( -0.4122572571062000368, 29.27166520044000109, -2.305209684642999690 ) ) ;
#22247 = CARTESIAN_POINT ( 'NONE',  ( 17.69733580085999947, -10.50304813760000044, -4.466741093449000388 ) ) ;
#22248 = CARTESIAN_POINT ( 'NONE',  ( -10.34021276376999943, -7.200000000000000178, -5.302007471952000326E-09 ) ) ;
#22249 = B_SPLINE_CURVE_WITH_KNOTS ( 'NONE', 3,
 ( #10429, #3283, #16222, #4981, #22118, #5637, #10665, #1339, #16090, #16660, #21568, #18053, #12904, #20304, #7450, #18483, #19756, #3832 ),
 .UNSPECIFIED., .F., .F.,
 ( 4, 2, 2, 2, 2, 2, 2, 2, 4 ),
 ( 0.000000000000000000, 0.1249999999999999722, 0.2500000000000000000, 0.3750000000000000000, 0.5000000000000001110, 0.6250000000000001110, 0.7500000000000000000, 0.8750000000000000000, 1.000000000000000000 ),
 .UNSPECIFIED. ) ;
#22250 = ORIENTED_EDGE ( 'NONE', *, *, #6277, .F. ) ;
#22251 = CARTESIAN_POINT ( 'NONE',  ( -2.500000000000000000, 28.80000000000000071, 0.000000000000000000 ) ) ;
#22252 = CARTESIAN_POINT ( 'NONE',  ( 18.88525750721999685, 2.047957541271999915, 10.33960724111999951 ) ) ;
#22253 = DIRECTION ( 'NONE',  ( 0.7071067811823850136, 0.7071067811898851252, 1.080116765722976056E-06 ) ) ;
#22254 = ORIENTED_EDGE ( 'NONE', *, *, #7702, .T. ) ;
#22255 = CARTESIAN_POINT ( 'NONE',  ( 13.72309434659665683, -9.869885134801844373, 3.116967400436540636 ) ) ;
#22256 = LINE ( 'NONE', #7250, #14160 ) ;
#22257 = CARTESIAN_POINT ( 'NONE',  ( -4.621291600221002049, 12.34015603868000710, 1.443184655503999547 ) ) ;
#22258 = CARTESIAN_POINT ( 'NONE',  ( 1.960055799040040236, 29.05894037691824394, -0.9073345561690950856 ) ) ;
#22259 = CARTESIAN_POINT ( 'NONE',  ( -20.47282685430000271, 1.064915000120000066, -11.01223998885000022 ) ) ;
#22260 = ORIENTED_EDGE ( 'NONE', *, *, #17403, .F. ) ;
#22261 = DIRECTION ( 'NONE',  ( -1.000000000000000000, 0.000000000000000000, 0.000000000000000000 ) ) ;
#22262 = ORIENTED_EDGE ( 'NONE', *, *, #23079, .F. ) ;
#22263 = B_SPLINE_CURVE_WITH_KNOTS ( 'NONE', 3,
 ( #8413, #13847, #10224, #2962 ),
 .UNSPECIFIED., .F., .F.,
 ( 4, 4 ),
 ( 0.000000000000000000, 1.000000000000000000 ),
 .UNSPECIFIED. ) ;
#22264 = CARTESIAN_POINT ( 'NONE',  ( -0.6416724176654999834, 23.68578163881999998, -2.183283362266000172 ) ) ;
#22265 = ADVANCED_FACE ( 'NONE', ( #23652, #10468 ), #21356, .T. ) ;
#22266 = CARTESIAN_POINT ( 'NONE',  ( 6.543402445986997051, 13.52098819050001133, 1.162556828447999901 ) ) ;
#22267 = CARTESIAN_POINT ( 'NONE',  ( 1.603022320644999832, 27.19049822781000003, 1.603022320644999832 ) ) ;
#22268 = FACE_OUTER_BOUND ( 'NONE', #16141, .T. ) ;
#22269 = ADVANCED_FACE ( 'NONE', ( #14443 ), #16520, .F. ) ;
#22270 = AXIS2_PLACEMENT_3D ( 'NONE', #11703, #4433, #23063 ) ;
#22271 = DIRECTION ( 'NONE',  ( 0.000000000000000000, -1.000000000000000000, 0.000000000000000000 ) ) ;
#22272 = FACE_OUTER_BOUND ( 'NONE', #5025, .T. ) ;
#22273 = CARTESIAN_POINT ( 'NONE',  ( 14.10412674931000154, -7.190271978224999749, -7.885398697387000944 ) ) ;
#22274 = DIRECTION ( 'NONE',  ( 0.5000000000000169864, 0.000000000000000000, 0.8660254037844289376 ) ) ;
#22275 = FACE_OUTER_BOUND ( 'NONE', #9676, .T. ) ;
#22276 = CARTESIAN_POINT ( 'NONE',  ( 6.750000000000000000, 27.79903810567699907, -6.000000000000000000 ) ) ;
#22277 = ORIENTED_EDGE ( 'NONE', *, *, #9802, .T. ) ;
#22278 = EDGE_CURVE ( 'NONE', #6193, #11323, #4140, .T. ) ;
#22279 = CARTESIAN_POINT ( 'NONE',  ( -18.73259798496000172, -8.620928137991000995, 3.072238420002000314 ) ) ;
#22280 = EDGE_CURVE ( 'NONE', #959, #20904, #21605, .T. ) ;
#22281 = CARTESIAN_POINT ( 'NONE',  ( -0.5541245210720000536, 24.21556899698000009, -2.268390014031999691 ) ) ;
#22282 = CARTESIAN_POINT ( 'NONE',  ( 14.73749136213059785, 8.405818844597368056, -6.030319882502336526 ) ) ;
#22283 = CARTESIAN_POINT ( 'NONE',  ( -18.48259587121333425, -7.991236091536491060, -4.606005739639033258 ) ) ;
#22284 = CARTESIAN_POINT ( 'NONE',  ( 23.28092879524999859, -10.85541562098999968, -3.071221882731999919 ) ) ;
#22285 = CARTESIAN_POINT ( 'NONE',  ( -2.135020154818999760, 29.15352773921999940, 1.400017537060999961 ) ) ;
#22286 = CARTESIAN_POINT ( 'NONE',  ( 14.31728336214042230, -1.911400327409435551, 8.862201799975091276 ) ) ;
#22287 = CARTESIAN_POINT ( 'NONE',  ( 3.779846905083999342, 12.27705807091000700, -3.020046618730999555 ) ) ;
#22288 = AXIS2_PLACEMENT_3D ( 'NONE', #16198, #15705, #5082 ) ;
#22289 = CARTESIAN_POINT ( 'NONE',  ( -2.500000000000000444, 26.65086340285667177, 0.3272492347489422415 ) ) ;
#22290 = AXIS2_PLACEMENT_3D ( 'NONE', #2600, #1274, #12301 ) ;
#22291 = CARTESIAN_POINT ( 'NONE',  ( 11.29022434643809270, 9.635153832122318462, -8.311371697084542376 ) ) ;
#22292 = ORIENTED_EDGE ( 'NONE', *, *, #1828, .F. ) ;
#22293 = CARTESIAN_POINT ( 'NONE',  ( 0.4737338993650556107, 24.45831145367538895, 2.488861676985053784 ) ) ;
#22294 = B_SPLINE_CURVE_WITH_KNOTS ( 'NONE', 3,
 ( #10100, #15778, #8038, #11799 ),
 .UNSPECIFIED., .F., .F.,
 ( 4, 4 ),
 ( 0.000000000000000000, 1.000000000000000000 ),
 .UNSPECIFIED. ) ;
#22295 = CARTESIAN_POINT ( 'NONE',  ( 2.218255378514000675, 23.92992329518563821, -1.026110373679216536 ) ) ;
#22296 = EDGE_LOOP ( 'NONE', ( #21411, #11854, #8239, #18137, #12543, #15363, #11708, #23678, #6614, #22454, #7896, #22870 ) ) ;
#22297 = CARTESIAN_POINT ( 'NONE',  ( 22.87199999999999989, 9.258222311379999070, 0.000000000000000000 ) ) ;
#22298 = DIRECTION ( 'NONE',  ( 0.000000000000000000, 0.000000000000000000, -1.000000000000000000 ) ) ;
#22299 = AXIS2_PLACEMENT_3D ( 'NONE', #22939, #17507, #6483 ) ;
#22300 = CARTESIAN_POINT ( 'NONE',  ( 17.51266765309999940, -10.43854800410000117, 3.769063558861000196 ) ) ;
#22301 = CARTESIAN_POINT ( 'NONE',  ( 13.50000000000000000, 4.517872873748999929, -7.804362139085999850 ) ) ;
#22302 = AXIS2_PLACEMENT_3D ( 'NONE', #11626, #19113, #15229 ) ;
#22303 = CARTESIAN_POINT ( 'NONE',  ( 1.304555153736000062, 25.61462896666999711, -2.329463490920999913 ) ) ;
#22304 = ORIENTED_EDGE ( 'NONE', *, *, #15572, .T. ) ;
#22305 = ORIENTED_EDGE ( 'NONE', *, *, #22539, .T. ) ;
#22306 = VECTOR ( 'NONE', #7553, 1000.000000000000114 ) ;
#22307 = CARTESIAN_POINT ( 'NONE',  ( -10.60714863877000091, 13.96228639389999948, -6.054349922818000884 ) ) ;
#22308 = CARTESIAN_POINT ( 'NONE',  ( 11.00000000000000000, 10.59999999999999964, 0.000000000000000000 ) ) ;
#22309 = LINE ( 'NONE', #2089, #7866 ) ;
#22310 = ORIENTED_EDGE ( 'NONE', *, *, #1640, .T. ) ;
#22311 = CARTESIAN_POINT ( 'NONE',  ( -24.48376588670982912, 10.31426502621302710, 7.135315508360969616 ) ) ;
#22312 = CARTESIAN_POINT ( 'NONE',  ( 20.14674727276818800, 10.50482826883816578, -0.4971117468655986138 ) ) ;
#22313 = LINE ( 'NONE', #9017, #14157 ) ;
#22314 = CARTESIAN_POINT ( 'NONE',  ( 15.89284332445408943, -10.06731258041612165, -2.433320157096150460 ) ) ;
#22315 = CARTESIAN_POINT ( 'NONE',  ( -18.19808584514999694, 4.666018550332999837, 10.07846247694000041 ) ) ;
#22316 = CARTESIAN_POINT ( 'NONE',  ( 1.349135513845000078, 29.14813513062999917, -1.722924400667999789 ) ) ;
#22317 = CARTESIAN_POINT ( 'NONE',  ( -13.19880458549999958, -0.9434914505904000714, -10.69878979702999899 ) ) ;
#22318 = PRODUCT_RELATED_PRODUCT_CATEGORY ( 'part', '', ( #20806 ) ) ;
#22319 = CARTESIAN_POINT ( 'NONE',  ( 0.9601661138225395797, 29.66260720285410812, 1.934687070640197737 ) ) ;
#22320 = ORIENTED_EDGE ( 'NONE', *, *, #13816, .T. ) ;
#22321 = TOROIDAL_SURFACE ( 'NONE', #17711, 4.649999999999999467, 0.1000000000000000056 ) ;
#22322 = CARTESIAN_POINT ( 'NONE',  ( -2.142313624094999813, 25.45688484113999905, 0.4115616050618999822 ) ) ;
#22323 = CARTESIAN_POINT ( 'NONE',  ( 20.89509018864575296, -2.982496466438095517, 10.10845216425653881 ) ) ;
#22324 = CARTESIAN_POINT ( 'NONE',  ( 4.816302164864996627, 14.93028961201002147, -3.795745731844999415 ) ) ;
#22325 = ORIENTED_EDGE ( 'NONE', *, *, #1343, .T. ) ;
#22326 = CARTESIAN_POINT ( 'NONE',  ( -23.74465998031000069, -7.716878364870000340, 11.63397459621999985 ) ) ;
#22327 = CARTESIAN_POINT ( 'NONE',  ( -4.498662548786000137, 15.01211498829999869, 3.843732114414002865 ) ) ;
#22328 = CARTESIAN_POINT ( 'NONE',  ( 18.18583333333330998, -7.984581761151016366, 4.602170423446800385 ) ) ;
#22329 = CARTESIAN_POINT ( 'NONE',  ( 13.03762625731000036, -8.686210121801000383, 2.766264305181999728 ) ) ;
#22330 = VERTEX_POINT ( 'NONE', #1373 ) ;
#22331 = VECTOR ( 'NONE', #17404, 1000.000000000000114 ) ;
#22332 = CARTESIAN_POINT ( 'NONE',  ( -4.623317570261906262, 15.59290886452487968, 4.017537324272654864 ) ) ;
#22333 = AXIS2_PLACEMENT_3D ( 'NONE', #1013, #17492, #23542 ) ;
#22334 = CARTESIAN_POINT ( 'NONE',  ( -14.25243324638999809, 6.216878364870000340, -12.50000000000000000 ) ) ;
#22335 = ORIENTED_EDGE ( 'NONE', *, *, #22345, .T. ) ;
#22336 = CARTESIAN_POINT ( 'NONE',  ( -23.13361993687182760, 5.790620044384096055, -7.422872665018464211 ) ) ;
#22337 = CARTESIAN_POINT ( 'NONE',  ( 1.591886459334999726, 11.74621052866999449, 4.486094747653003978 ) ) ;
#22338 = CARTESIAN_POINT ( 'NONE',  ( -23.26061350940999972, 3.997618465669000365, -8.779111753320000489 ) ) ;
#22339 = CARTESIAN_POINT ( 'NONE',  ( -14.41332696916413525, 9.018101604870871313, -9.380024591087739338 ) ) ;
#22340 = CARTESIAN_POINT ( 'NONE',  ( -4.696142548075968648, 13.41911879355214410, 5.316338907189500418 ) ) ;
#22341 = CARTESIAN_POINT ( 'NONE',  ( -19.73799724739764727, -5.961347995097865393, 8.625741937770200707 ) ) ;
#22342 = CARTESIAN_POINT ( 'NONE',  ( 0.000000000000000000, -1.550000000000000044, 0.000000000000000000 ) ) ;
#22343 = FILL_AREA_STYLE_COLOUR ( '', #13077 ) ;
#22344 = PLANE ( 'NONE',  #7603 ) ;
#22345 = EDGE_CURVE ( 'NONE', #16051, #21619, #20546, .T. ) ;
#22346 = CARTESIAN_POINT ( 'NONE',  ( 2.022356098371595134, 30.55380357660929747, 0.8395515573483458560 ) ) ;
#22347 = EDGE_LOOP ( 'NONE', ( #1802, #9437, #7180, #5200 ) ) ;
#22348 = CARTESIAN_POINT ( 'NONE',  ( -18.14837077250665942, -7.306469912381244214, -5.615206019344828547 ) ) ;
#22349 = CARTESIAN_POINT ( 'NONE',  ( 24.47854514379999813, -6.961171424654001072, -6.740760433291000275 ) ) ;
#22350 = CARTESIAN_POINT ( 'NONE',  ( -2.143277222256999792, 23.64327722226000006, 4.118360636503000477E-13 ) ) ;
#22351 = CARTESIAN_POINT ( 'NONE',  ( 4.750000000000000000, 22.00000000000000000, 0.000000000000000000 ) ) ;
#22352 = AXIS2_PLACEMENT_3D ( 'NONE', #23653, #7060, #12859 ) ;
#22353 = CARTESIAN_POINT ( 'NONE',  ( -23.40224104270576433, 2.202070123285927217, 10.35029114405029915 ) ) ;
#22354 = CARTESIAN_POINT ( 'NONE',  ( 1.854615231836999945, 26.30864211382000306, 1.347456777940000183 ) ) ;
#22355 = CARTESIAN_POINT ( 'NONE',  ( -2.131902921039358745, 30.85616845379279383, 0.2258430825467815373 ) ) ;
#22356 = CARTESIAN_POINT ( 'NONE',  ( 3.126566019963172405, 11.89425924942375090, 3.678199694141997877 ) ) ;
#22357 = VERTEX_POINT ( 'NONE', #7402 ) ;
#22358 = TOROIDAL_SURFACE ( 'NONE', #21608, 2.500000000000000000, 0.5500000000000000444 ) ;
#22359 = VECTOR ( 'NONE', #15340, 1000.000000000000114 ) ;
#22360 = CARTESIAN_POINT ( 'NONE',  ( -2.274037557443177260, 11.70145862779804347, -4.252662107751031151 ) ) ;
#22361 = ADVANCED_FACE ( 'NONE', ( #16487 ), #14215, .F. ) ;
#22362 = CARTESIAN_POINT ( 'NONE',  ( -3.643546194520566051, 29.79977277844448125, 2.515199777306227347 ) ) ;
#22363 = AXIS2_PLACEMENT_3D ( 'NONE', #890, #1015, #20889 ) ;
#22364 = DIRECTION ( 'NONE',  ( 0.000000000000000000, 0.7071067811866525998, -0.7071067811864425456 ) ) ;
#22365 = ORIENTED_EDGE ( 'NONE', *, *, #477, .T. ) ;
#22366 = DIRECTION ( 'NONE',  ( 0.000000000000000000, -1.000000000000000000, 0.000000000000000000 ) ) ;
#22367 = AXIS2_PLACEMENT_3D ( 'NONE', #5143, #3665, #9350 ) ;
#22368 = CARTESIAN_POINT ( 'NONE',  ( 13.74862658530999937, -9.135377135809001459, -4.430325866828999537 ) ) ;
#22369 = DIRECTION ( 'NONE',  ( 0.000000000000000000, 1.000000000000000000, 0.000000000000000000 ) ) ;
#22370 = CARTESIAN_POINT ( 'NONE',  ( -1.200923599098000061, 28.00000000000000000, 5.906307787036999990 ) ) ;
#22371 = CARTESIAN_POINT ( 'NONE',  ( 18.57801537305999773, 8.813863540509998984, -6.409915686984000160 ) ) ;
#22372 = CARTESIAN_POINT ( 'NONE',  ( -1.657661551580862591, 30.87634082601233132, -1.328962299251567059 ) ) ;
#22373 = ORIENTED_EDGE ( 'NONE', *, *, #16778, .F. ) ;
#22374 = CARTESIAN_POINT ( 'NONE',  ( -4.000000000000000000, 29.69999999999999929, -2.309401076759000304 ) ) ;
#22375 = CARTESIAN_POINT ( 'NONE',  ( 23.40574053114000108, -10.02401005856000005, -4.063832034710999963 ) ) ;
#22376 = AXIS2_PLACEMENT_3D ( 'NONE', #2156, #2512, #3980 ) ;
#22377 = EDGE_CURVE ( 'NONE', #16006, #6468, #18238, .T. ) ;
#22378 = CARTESIAN_POINT ( 'NONE',  ( 3.821520914465098784, 29.74995697614778578, 2.412446024836691461 ) ) ;
#22379 = EDGE_LOOP ( 'NONE', ( #8014, #19622, #512, #18707 ) ) ;
#22380 = CARTESIAN_POINT ( 'NONE',  ( 18.22028936713000036, -1.652712406954000013, 8.988165862088999702 ) ) ;
#22381 = CARTESIAN_POINT ( 'NONE',  ( 24.50000000000000000, 8.054858440593999802, 5.882793087032000656 ) ) ;
#22382 = CARTESIAN_POINT ( 'NONE',  ( 4.796469116184001180, 12.40727786077000161, 0.6646592000246001053 ) ) ;
#22383 = CARTESIAN_POINT ( 'NONE',  ( 1.982538622003251705, 29.05572842088777463, -0.8582355642374253080 ) ) ;
#22384 = CARTESIAN_POINT ( 'NONE',  ( -21.76857732275000146, 2.577874773493999516, 10.79524278768000123 ) ) ;
#22385 = ORIENTED_EDGE ( 'NONE', *, *, #12227, .T. ) ;
#22386 = B_SPLINE_CURVE_WITH_KNOTS ( 'NONE', 3,
 ( #8448, #3917, #5845, #11425, #14916, #18798, #18685, #4148, #15155, #22549 ),
 .UNSPECIFIED., .F., .F.,
 ( 4, 2, 2, 2, 4 ),
 ( 0.000000000000000000, 0.2500000000000000000, 0.5000000000000000000, 0.7500000000000000000, 1.000000000000000000 ),
 .UNSPECIFIED. ) ;
#22387 = CARTESIAN_POINT ( 'NONE',  ( 1.699997194034733150, 11.63334146140299907, 1.053569902902707689 ) ) ;
#22388 = AXIS2_PLACEMENT_3D ( 'NONE', #15559, #15803, #13746 ) ;
#22389 = ORIENTED_EDGE ( 'NONE', *, *, #16712, .T. ) ;
#22390 = CARTESIAN_POINT ( 'NONE',  ( 0.8867402482005000142, 25.08986973128999765, -1.970974702784000110 ) ) ;
#22391 = CARTESIAN_POINT ( 'NONE',  ( 5.818048057449997756, 13.71143573768000223, 3.214928120249999299 ) ) ;
#22393 = EDGE_CURVE ( 'NONE', #3216, #14191, #7234, .T. ) ;
#22392 = CARTESIAN_POINT ( 'NONE',  ( 0.4858445502738999999, 28.26299822781000159, -2.214344957515000267 ) ) ;
#22394 = CARTESIAN_POINT ( 'NONE',  ( 15.90028936713000185, 9.079314476020000413, 0.000000000000000000 ) ) ;
#22395 = DIRECTION ( 'NONE',  ( 1.000000000000000000, 0.000000000000000000, 0.000000000000000000 ) ) ;
#22396 = DIRECTION ( 'NONE',  ( 0.000000000000000000, -1.000000000000000000, 0.000000000000000000 ) ) ;
#22397 = DIRECTION ( 'NONE',  ( 0.000000000000000000, -1.000000000000000000, 0.000000000000000000 ) ) ;
#22398 = AXIS2_PLACEMENT_3D ( 'NONE', #8246, #17320, #6660 ) ;
#22399 = CARTESIAN_POINT ( 'NONE',  ( -16.04262945707999677, 5.313593037366000082, 9.424424275870000756 ) ) ;
#22400 = AXIS2_PLACEMENT_3D ( 'NONE', #5297, #14608, #22004 ) ;
#22401 = DIRECTION ( 'NONE',  ( -1.000000000000000000, 0.000000000000000000, 0.000000000000000000 ) ) ;
#22402 = CONICAL_SURFACE ( 'NONE', #16219, 7.249999994591000529, 0.7853981633972997312 ) ;
#22403 = EDGE_CURVE ( 'NONE', #9506, #9908, #10349, .T. ) ;
#22404 = CARTESIAN_POINT ( 'NONE',  ( -14.47158022755693985, -2.069973096218738373, 12.49996948346097092 ) ) ;
#22405 = EDGE_LOOP ( 'NONE', ( #8925, #3481, #12815, #17437 ) ) ;
#22406 = CARTESIAN_POINT ( 'NONE',  ( -10.53831236658635007, 15.50609459400975609, -1.406661532941654080 ) ) ;
#22407 = CARTESIAN_POINT ( 'NONE',  ( 1.327909667750000189, 24.70915199424000264, -2.369304801069999744 ) ) ;
#22408 = CARTESIAN_POINT ( 'NONE',  ( 14.37355788048617100, -3.089454521824534616, -9.852699315173421013 ) ) ;
#22409 = DIRECTION ( 'NONE',  ( 0.000000000000000000, -0.7071067811866525998, -0.7071067811864425456 ) ) ;
#22410 = CARTESIAN_POINT ( 'NONE',  ( 21.66593149462999790, -1.098770618442999947, -11.18333031146000067 ) ) ;
#22411 = ADVANCED_FACE ( 'NONE', ( #13849 ), #4534, .T. ) ;
#22412 = CARTESIAN_POINT ( 'NONE',  ( -0.9467533411658000109, 29.72799882400999749, -2.371079559876999809 ) ) ;
#22413 = CARTESIAN_POINT ( 'NONE',  ( 14.08726172903277707, 4.895756663341041204, 7.589951152256699807 ) ) ;
#22414 = ADVANCED_FACE ( 'NONE', ( #17243 ), #12286, .T. ) ;
#22415 = CARTESIAN_POINT ( 'NONE',  ( 17.87679683445078638, -0.5884589777194313420, -10.44048563999592538 ) ) ;
#22416 = AXIS2_PLACEMENT_3D ( 'NONE', #9893, #22369, #437 ) ;
#22417 = CARTESIAN_POINT ( 'NONE',  ( 11.48696334737753055, 12.46086172548929838, -3.416997251963662219 ) ) ;
#22418 = ORIENTED_EDGE ( 'NONE', *, *, #22450, .T. ) ;
#22419 = CARTESIAN_POINT ( 'NONE',  ( 13.50000000000000000, 0.000000000000000000, 0.000000000000000000 ) ) ;
#22420 = EDGE_LOOP ( 'NONE', ( #14591, #4408, #13277, #10494 ) ) ;
#22421 = DIRECTION ( 'NONE',  ( -1.000000000000000000, 0.000000000000000000, 0.000000000000000000 ) ) ;
#22422 = CARTESIAN_POINT ( 'NONE',  ( 2.500000000000000000, 27.83419673618999823, 0.000000000000000000 ) ) ;
#22423 = ADVANCED_FACE ( 'NONE', ( #19310, #2964 ), #17368, .T. ) ;
#22424 = CARTESIAN_POINT ( 'NONE',  ( -3.316026328260925471, 28.13336607546986556, -2.704152903936609231 ) ) ;
#22425 = AXIS2_PLACEMENT_3D ( 'NONE', #6290, #13921, #15848 ) ;
#22426 = CARTESIAN_POINT ( 'NONE',  ( 17.15176585740999826, 0.2857122287928000048, 11.08459265502000157 ) ) ;
#22427 = DIRECTION ( 'NONE',  ( 0.000000000000000000, 0.7071067811866525998, -0.7071067811864425456 ) ) ;
#22428 = CARTESIAN_POINT ( 'NONE',  ( 1.887779699469000150, 26.97962896666999910, 1.887779699469000150 ) ) ;
#22429 = ORIENTED_EDGE ( 'NONE', *, *, #14246, .T. ) ;
#22430 = ORIENTED_EDGE ( 'NONE', *, *, #21571, .F. ) ;
#22431 = CARTESIAN_POINT ( 'NONE',  ( -9.683372211694999621, -6.488719643906999401, -14.15222824137000046 ) ) ;
#22432 = DIRECTION ( 'NONE',  ( -9.309572557292000170E-11, 0.000000000000000000, 1.000000000000000000 ) ) ;
#22433 = CARTESIAN_POINT ( 'NONE',  ( 18.05162270046333717, 3.606460571753791644, 8.497838180424565735 ) ) ;
#22434 = VERTEX_POINT ( 'NONE', #643 ) ;
#22435 = CARTESIAN_POINT ( 'NONE',  ( -14.49863740983932914, 10.56606202786612059, 6.698971014615676900 ) ) ;
#22436 = CARTESIAN_POINT ( 'NONE',  ( 19.79377223792668161, 3.114699025246350672, -10.03687850954299243 ) ) ;
#22437 = DIRECTION ( 'NONE',  ( 0.000000000000000000, 0.000000000000000000, 1.000000000000000000 ) ) ;
#22438 = CARTESIAN_POINT ( 'NONE',  ( 15.75498143486384706, -10.05429136305618165, 2.469775658380014782 ) ) ;
#22439 = CARTESIAN_POINT ( 'NONE',  ( -18.23212756329999706, 9.685834697697000450, 5.436217751806999843 ) ) ;
#22440 = CARTESIAN_POINT ( 'NONE',  ( -1.020771968315000056, 30.12698763284999970, 1.940619092743999907 ) ) ;
#22441 = CARTESIAN_POINT ( 'NONE',  ( -18.92721240987999920, -2.665110294750000275, -11.12003873501999962 ) ) ;
#22442 = CARTESIAN_POINT ( 'NONE',  ( 1.417757377811232677, 29.69484876337556045, 1.629552333889765281 ) ) ;
#22443 = ORIENTED_EDGE ( 'NONE', *, *, #14408, .F. ) ;
#22444 = CARTESIAN_POINT ( 'NONE',  ( -0.6125396999611999460, 25.59648037213999672, 2.093726834476999699 ) ) ;
#22445 = CARTESIAN_POINT ( 'NONE',  ( -24.50000000000000000, -3.090136434824279466, -10.17978739575026381 ) ) ;
#22446 = CARTESIAN_POINT ( 'NONE',  ( 4.649999999999999467, 20.10000000000000142, -5.428584221033999407E-09 ) ) ;
#22447 = ORIENTED_EDGE ( 'NONE', *, *, #751, .T. ) ;
#22448 = CARTESIAN_POINT ( 'NONE',  ( -1.989999999999999991, 12.34057940292999866, 0.000000000000000000 ) ) ;
#22449 = CARTESIAN_POINT ( 'NONE',  ( -4.810176010396001622, 16.11838285530999926, 3.920675986495997911 ) ) ;
#22450 = EDGE_CURVE ( 'NONE', #9818, #4666, #19634, .T. ) ;
#22451 = EDGE_CURVE ( 'NONE', #15250, #14519, #6703, .T. ) ;
#22452 = DIRECTION ( 'NONE',  ( 0.000000000000000000, -0.8660254037844288266, 0.5000000000000169864 ) ) ;
#22453 = CARTESIAN_POINT ( 'NONE',  ( 11.31918875731000007, -8.923818741964000267, -0.1967739533420000131 ) ) ;
#22454 = ORIENTED_EDGE ( 'NONE', *, *, #3763, .F. ) ;
#22455 = FACE_OUTER_BOUND ( 'NONE', #4937, .T. ) ;
#22456 = DIRECTION ( 'NONE',  ( 0.000000000000000000, 0.000000000000000000, -1.000000000000000000 ) ) ;
#22457 = ORIENTED_EDGE ( 'NONE', *, *, #4509, .T. ) ;
#22458 = DIRECTION ( 'NONE',  ( 0.000000000000000000, 1.000000000000000000, 0.000000000000000000 ) ) ;
#22459 = CARTESIAN_POINT ( 'NONE',  ( 3.100000000000000089, 20.00000000000000000, 0.000000000000000000 ) ) ;
#22460 = CARTESIAN_POINT ( 'NONE',  ( -1.915921331177998788, 11.82052783618998681, 4.443859913084001967 ) ) ;
#22461 = CIRCLE ( 'NONE', #17050, 12.44999999999999929 ) ;
#22462 = CARTESIAN_POINT ( 'NONE',  ( 12.00000000000000000, 0.4049267614696120399, -9.310983403904009137 ) ) ;
#22463 = CARTESIAN_POINT ( 'NONE',  ( 4.624999963076000142, 12.99999996307999872, 4.214403195776000249E-08 ) ) ;
#22464 = CARTESIAN_POINT ( 'NONE',  ( -5.062275720949998004, 15.74663350384999028, -2.895383246133002242 ) ) ;
#22465 = CARTESIAN_POINT ( 'NONE',  ( -2.000000000000000000, 26.50000000000000355, -3.464101615137999968 ) ) ;
#22466 = CARTESIAN_POINT ( 'NONE',  ( 5.205597908719371780, 13.92591030125720231, -4.046157760719942154 ) ) ;
#22467 = CARTESIAN_POINT ( 'NONE',  ( 1.536366799937286087, 27.95086340285666537, -1.999167105995451221 ) ) ;
#22468 = CARTESIAN_POINT ( 'NONE',  ( -0.8956276177791392401, 30.34935011684900985, 1.967630924038994422 ) ) ;
#22469 = EDGE_LOOP ( 'NONE', ( #12514, #1852, #9243 ) ) ;
#22470 = CARTESIAN_POINT ( 'NONE',  ( -17.35474577250666783, 8.879308410214960645, 2.386378174953934561 ) ) ;
#22471 = DIRECTION ( 'NONE',  ( -0.000000000000000000, 1.000000000000000000, 0.000000000000000000 ) ) ;
#22472 = CARTESIAN_POINT ( 'NONE',  ( 4.335853037485340344, 13.43036814054341122, -5.287594306914102482 ) ) ;
#22473 = CARTESIAN_POINT ( 'NONE',  ( 0.000000000000000000, 0.000000000000000000, 0.000000000000000000 ) ) ;
#22474 = CARTESIAN_POINT ( 'NONE',  ( -21.09947279093694661, -10.48387386659816656, 0.9232800561193126310 ) ) ;
#22475 = FACE_OUTER_BOUND ( 'NONE', #8320, .T. ) ;
#22476 = CARTESIAN_POINT ( 'NONE',  ( 12.50000000000000000, 13.93375672974000068, 0.000000000000000000 ) ) ;
#22477 = VERTEX_POINT ( 'NONE', #13725 ) ;
#22478 = CARTESIAN_POINT ( 'NONE',  ( -17.74018339386138265, -5.574914795658462374, 8.993144632062060495 ) ) ;
#22479 = CARTESIAN_POINT ( 'NONE',  ( -2.944270284434496787, 29.92936170367566717, 2.918926912232259419 ) ) ;
#22480 = CARTESIAN_POINT ( 'NONE',  ( -4.000024251878890880, 28.02555747447231127, 0.7498250608958049179 ) ) ;
#22481 = ORIENTED_EDGE ( 'NONE', *, *, #1069, .F. ) ;
#22482 = EDGE_CURVE ( 'NONE', #16467, #6064, #21123, .T. ) ;
#22483 = DIRECTION ( 'NONE',  ( -0.9996708941621513800, 0.02565352539212875996, -2.108144717745900797E-14 ) ) ;
#22484 = CARTESIAN_POINT ( 'NONE',  ( 15.83268908530999930, -1.865934471007999917, -10.03576702404999921 ) ) ;
#22485 = LINE ( 'NONE', #2631, #14285 ) ;
#22486 = DIRECTION ( 'NONE',  ( 0.9996708941621511579, -0.02565352539213875543, 2.155425419848895702E-14 ) ) ;
#22487 = CARTESIAN_POINT ( 'NONE',  ( 15.73426537305999950, -5.346007409990000347, 9.405856311918000756 ) ) ;
#22488 = CARTESIAN_POINT ( 'NONE',  ( -0.8612498596054259936, 30.84999136413794218, -1.988030992341762504 ) ) ;
#22489 = DIRECTION ( 'NONE',  ( -2.979866527141999703E-10, 1.005728194337683875E-23, 1.000000000000000000 ) ) ;
#22490 = CARTESIAN_POINT ( 'NONE',  ( 24.73933971626999906, 6.229381467500999747, 8.232746011927000396 ) ) ;
#22491 = TOROIDAL_SURFACE ( 'NONE', #15522, 14.44999999999999929, 2.000000000000000000 ) ;
#22492 = CARTESIAN_POINT ( 'NONE',  ( 23.99895687519700616, 13.93375672973999890, 0.3849913041842834560 ) ) ;
#22493 = ORIENTED_EDGE ( 'NONE', *, *, #10737, .F. ) ;
#22494 = CARTESIAN_POINT ( 'NONE',  ( 12.15527934810000055, -8.048449879512999061, -4.237977357754999730 ) ) ;
#22495 = DIRECTION ( 'NONE',  ( 0.4226182617407188702, 0.000000000000000000, 0.9063077870366409439 ) ) ;
#22496 = CARTESIAN_POINT ( 'NONE',  ( -3.969064160570000777, 12.18274565056999847, 2.680101174410998155 ) ) ;
#22497 = DIRECTION ( 'NONE',  ( -1.000000000000000000, 0.000000000000000000, 0.000000000000000000 ) ) ;
#22498 = CARTESIAN_POINT ( 'NONE',  ( -24.27484550945999686, 5.445138765948000170, -9.749175221210998998 ) ) ;
#22499 = ORIENTED_EDGE ( 'NONE', *, *, #7717, .T. ) ;
#22500 = CARTESIAN_POINT ( 'NONE',  ( -18.94247183136150525, -9.023122249501957626, 3.215535042062015680 ) ) ;
#22501 = CIRCLE ( 'NONE', #7050, 2.270871215252209030 ) ;
#22502 = ORIENTED_EDGE ( 'NONE', *, *, #7163, .F. ) ;
#22503 = CARTESIAN_POINT ( 'NONE',  ( 15.48458103379664941, 1.186956113863779416, -9.068646580869270224 ) ) ;
#22504 = CARTESIAN_POINT ( 'NONE',  ( 6.633606867079997471, 13.50105012196000231, 0.4122077612039000694 ) ) ;
#22505 = CARTESIAN_POINT ( 'NONE',  ( -2.193530619437999984, 28.45799822781000188, -0.5724186824819998964 ) ) ;
#22506 = DIRECTION ( 'NONE',  ( 0.000000000000000000, 1.000000000000000000, 0.000000000000000000 ) ) ;
#22507 = DIRECTION ( 'NONE',  ( 0.000000000000000000, 0.000000000000000000, 1.000000000000000000 ) ) ;
#22508 = CARTESIAN_POINT ( 'NONE',  ( 17.06568924931000097, -1.008082813539000089, 10.70191082552000061 ) ) ;
#22509 = EDGE_CURVE ( 'NONE', #9620, #5222, #18462, .T. ) ;
#22510 = CARTESIAN_POINT ( 'NONE',  ( 0.000000000000000000, 0.000000000000000000, 0.000000000000000000 ) ) ;
#22511 = CARTESIAN_POINT ( 'NONE',  ( -15.23010806520000138, -8.044096712135001326, -7.201187562783000651 ) ) ;
#22512 = AXIS2_PLACEMENT_3D ( 'NONE', #3537, #10920, #16111 ) ;
#22513 = DIRECTION ( 'NONE',  ( 0.000000000000000000, 1.000000000000000000, 0.000000000000000000 ) ) ;
#22514 = CARTESIAN_POINT ( 'NONE',  ( -14.25243324638999809, -6.216878364870000340, 12.50000000000000000 ) ) ;
#22515 = ORIENTED_EDGE ( 'NONE', *, *, #20442, .T. ) ;
#22516 = PRESENTATION_STYLE_ASSIGNMENT (( #3999 ) ) ;
#22517 = CARTESIAN_POINT ( 'NONE',  ( 2.478439802523999980, 25.45499776881999665, 0.4854719611819000580 ) ) ;
#22518 = CARTESIAN_POINT ( 'NONE',  ( 13.84684978381418041, -8.707682685158594893, 5.508672335018611754 ) ) ;
#22519 = DIRECTION ( 'NONE',  ( 1.000000000000000000, 0.000000000000000000, 0.000000000000000000 ) ) ;
#22520 = SURFACE_STYLE_FILL_AREA ( #2795 ) ;
#22521 = SHAPE_REPRESENTATION ( 'MAS-673 Main Body', ( #4390 ), #7088 ) ;
#22522 = CARTESIAN_POINT ( 'NONE',  ( -0.8235893797016999862, 28.43543888322000157, 2.276936129739000059 ) ) ;
#22523 = EDGE_CURVE ( 'NONE', #2273, #13340, #4945, .T. ) ;
#22524 = CARTESIAN_POINT ( 'NONE',  ( 11.22285964975863237, -2.000465806332258456, 12.49999014999633573 ) ) ;
#22525 = DIRECTION ( 'NONE',  ( 0.000000000000000000, 1.000000000000000000, 0.000000000000000000 ) ) ;
#22526 = CARTESIAN_POINT ( 'NONE',  ( -6.399639659233631761, 15.54095944911451888, 1.345865623129033795 ) ) ;
#22527 = CARTESIAN_POINT ( 'NONE',  ( 0.6543697108981985089, 29.60086340285667461, -2.434931691670790599 ) ) ;
#22528 = ORIENTED_EDGE ( 'NONE', *, *, #5257, .F. ) ;
#22529 = AXIS2_PLACEMENT_3D ( 'NONE', #2173, #22401, #22055 ) ;
#22530 = CARTESIAN_POINT ( 'NONE',  ( 12.00000000000000000, -7.500000000000000000, 0.000000000000000000 ) ) ;
#22531 = EDGE_CURVE ( 'NONE', #9729, #12880, #8015, .T. ) ;
#22532 = ORIENTED_EDGE ( 'NONE', *, *, #12784, .F. ) ;
#22533 = CARTESIAN_POINT ( 'NONE',  ( -0.3396743697608000101, 25.47584390253999942, -2.715985394886999860 ) ) ;
#22534 = CARTESIAN_POINT ( 'NONE',  ( 24.32802197706126179, 9.050607035110887821, 9.323888775846091548 ) ) ;
#22535 = FACE_BOUND ( 'NONE', #15118, .T. ) ;
#22536 = ORIENTED_EDGE ( 'NONE', *, *, #21523, .F. ) ;
#22537 = CARTESIAN_POINT ( 'NONE',  ( 15.16680598110999867, 6.392462273583999988, 8.993531204449999095 ) ) ;
#22538 = DIRECTION ( 'NONE',  ( 1.000000000000000000, 0.000000000000000000, 0.000000000000000000 ) ) ;
#22539 = EDGE_CURVE ( 'NONE', #20510, #551, #6266, .T. ) ;
#22540 = CARTESIAN_POINT ( 'NONE',  ( -2.276308483783000103, 25.80962896666999740, -1.394936847711000016 ) ) ;
#22541 = ORIENTED_EDGE ( 'NONE', *, *, #1797, .T. ) ;
#22542 = ORIENTED_EDGE ( 'NONE', *, *, #15295, .F. ) ;
#22543 = CARTESIAN_POINT ( 'NONE',  ( -24.41904027018788526, 9.801083277732518084, -8.024000955001664437 ) ) ;
#22544 = CARTESIAN_POINT ( 'NONE',  ( 12.52688711657000020, 7.716878364870000340, 11.63397459621999985 ) ) ;
#22545 = DIRECTION ( 'NONE',  ( -0.5000000000000169864, 0.000000000000000000, -0.8660254037844288266 ) ) ;
#22546 = CARTESIAN_POINT ( 'NONE',  ( -23.86847083084956722, -7.985699633923855068, -11.16836250006485010 ) ) ;
#22547 = ORIENTED_EDGE ( 'NONE', *, *, #9047, .T. ) ;
#22548 = CARTESIAN_POINT ( 'NONE',  ( -22.68728007704000049, 0.8272991724924000367, 9.664718538323999297 ) ) ;
#22549 = CARTESIAN_POINT ( 'NONE',  ( 19.75000000000000000, -1.659811535170000019, 9.026773995975998943 ) ) ;
#22550 = ORIENTED_EDGE ( 'NONE', *, *, #13548, .F. ) ;
#22551 = CARTESIAN_POINT ( 'NONE',  ( 6.229047772746363343, 13.74469652872262415, 1.373019302850102985 ) ) ;
#22552 = CARTESIAN_POINT ( 'NONE',  ( 15.66899429073552774, -8.904753597334295279, 5.276170738670112215 ) ) ;
#22553 = CARTESIAN_POINT ( 'NONE',  ( -15.55621955597000117, -10.90559009245999889, 1.677215861521999862 ) ) ;
#22554 = CARTESIAN_POINT ( 'NONE',  ( 0.2174393203624000181, 28.97599530207000029, -2.181902348697000171 ) ) ;
#22555 = EDGE_CURVE ( 'NONE', #17452, #10425, #20217, .T. ) ;
#22556 = AXIS2_PLACEMENT_3D ( 'NONE', #21094, #14070, #3186 ) ;
#22557 = CARTESIAN_POINT ( 'NONE',  ( -18.27706328473999875, 10.02730951802000092, -4.225925492466999778 ) ) ;
#22558 = CARTESIAN_POINT ( 'NONE',  ( 0.6136530736515161122, 29.64045887480123653, 2.071129839369229675 ) ) ;
#22559 = ORIENTED_EDGE ( 'NONE', *, *, #5201, .T. ) ;
#22560 = CARTESIAN_POINT ( 'NONE',  ( 2.296839136161000106, 25.59511910883000141, 0.4914911606428001289 ) ) ;
#22561 = CARTESIAN_POINT ( 'NONE',  ( 2.270871215252209030, 19.00000000000000000, 0.000000000000000000 ) ) ;
#22562 = DIRECTION ( 'NONE',  ( -4.066191827689660386E-11, -1.000000000000000000, 0.000000000000000000 ) ) ;
#22563 = ORIENTED_EDGE ( 'NONE', *, *, #8627, .F. ) ;
#22564 = DIRECTION ( 'NONE',  ( 0.000000000000000000, -1.000000000000000000, 0.000000000000000000 ) ) ;
#22565 = CARTESIAN_POINT ( 'NONE',  ( -12.50000000000000000, 6.606768802097000126, -6.099810110451000966 ) ) ;
#22566 = CARTESIAN_POINT ( 'NONE',  ( -23.50032910583999879, 3.801543240379000377, -8.459419100777001432 ) ) ;
#22567 = EDGE_CURVE ( 'NONE', #2558, #21421, #14741, .T. ) ;
#22568 = CARTESIAN_POINT ( 'NONE',  ( 14.79262625730999936, -7.984278194804999451, 4.494107504349000415 ) ) ;
#22569 = ADVANCED_FACE ( 'NONE', ( #14344 ), #14223, .T. ) ;
#22570 = EDGE_LOOP ( 'NONE', ( #22304, #848, #21207, #6340 ) ) ;
#22571 = B_SPLINE_CURVE_WITH_KNOTS ( 'NONE', 3,
 ( #2745, #17514, #908, #4686, #12072, #1166, #19455, #17637, #1035, #23195, #6611, #21389, #4804, #2985, #15316, #12550, #18347, #7198, #18002, #10854, #18236 ),
 .UNSPECIFIED., .F., .F.,
 ( 4, 1, 1, 1, 1, 1, 1, 1, 1, 1, 1, 1, 1, 1, 1, 1, 1, 1, 4 ),
 ( 0.4517522507388516129, 0.4675004193362445881, 0.5000002515996020414, 0.5325000838631117617, 0.5649999161264690484, 0.5974997483898265571, 0.6299995806531840659, 0.6624994129165413526, 0.6949992451800510729, 0.7274990774434085816, 0.7599989097067658683, 0.7924987419701232660, 0.8249985742334806638, 0.8574984064968381725, 0.8899982387603480039, 0.9224980710237052905, 0.9549979032870627993, 0.9874977355504200860, 1.000000000000000000 ),
 .UNSPECIFIED. ) ;
#22572 = FACE_OUTER_BOUND ( 'NONE', #23396, .T. ) ;
#22573 = CARTESIAN_POINT ( 'NONE',  ( 0.000000000000000000, 21.94999982584599962, 0.000000000000000000 ) ) ;
#22574 = ORIENTED_EDGE ( 'NONE', *, *, #1873, .F. ) ;
#22575 = CARTESIAN_POINT ( 'NONE',  ( -16.06392920454665685, 7.937099294806711391, -4.574512672171699990 ) ) ;
#22576 = FACE_OUTER_BOUND ( 'NONE', #1671, .T. ) ;
#22577 = CARTESIAN_POINT ( 'NONE',  ( -4.760513096662999821, 12.62269162836001435, 0.7405673987019998350 ) ) ;
#22578 = CARTESIAN_POINT ( 'NONE',  ( -13.99999999999999467, -5.371542361985429892, 8.544981476852292701 ) ) ;
#22579 = CARTESIAN_POINT ( 'NONE',  ( 12.00000000000000178, 2.542583502621673208, -8.834538564857254528 ) ) ;
#22580 = LINE ( 'NONE', #653, #4514 ) ;
#22582 = ADVANCED_FACE ( 'NONE', ( #10836 ), #9761, .T. ) ;
#22581 = FACE_OUTER_BOUND ( 'NONE', #4295, .T. ) ;
#22583 = ADVANCED_FACE ( 'NONE', ( #10480 ), #21736, .T. ) ;
#22584 = CARTESIAN_POINT ( 'NONE',  ( 6.243179582884000212, 13.63341776306000064, 1.952383140737000033 ) ) ;
#22585 = CARTESIAN_POINT ( 'NONE',  ( 2.000000000000000000, 26.50000000000000355, -3.464101615137999968 ) ) ;
#22586 = CARTESIAN_POINT ( 'NONE',  ( -1.259047450927251788, 28.10086340285667106, -2.184465970885643316 ) ) ;
#22587 = CARTESIAN_POINT ( 'NONE',  ( 0.9083774594092118848, 30.45919981329474879, 1.959565387789651059 ) ) ;
#22588 = ORIENTED_EDGE ( 'NONE', *, *, #23253, .F. ) ;
#22589 = CARTESIAN_POINT ( 'NONE',  ( -11.04281598264000053, 15.31903517202000131, -1.878299281600999793 ) ) ;
#22590 = CARTESIAN_POINT ( 'NONE',  ( -0.5127195001119165818, 12.81264167692682143, -6.646073094678516924 ) ) ;
#22591 = DIRECTION ( 'NONE',  ( 1.000000000000000000, 0.000000000000000000, 0.000000000000000000 ) ) ;
#22592 = CARTESIAN_POINT ( 'NONE',  ( -21.26013104105991758, -8.417803719024050224, 6.324359816153899416 ) ) ;
#22593 = DIRECTION ( 'NONE',  ( 0.000000000000000000, 1.000000000000000000, 0.000000000000000000 ) ) ;
#22594 = CIRCLE ( 'NONE', #19903, 2.750000000000000000 ) ;
#22595 = CARTESIAN_POINT ( 'NONE',  ( -0.1752525090037950484, 28.25094615491813599, 4.517620070267612142 ) ) ;
#22596 = ORIENTED_EDGE ( 'NONE', *, *, #19951, .F. ) ;
#22597 = CARTESIAN_POINT ( 'NONE',  ( -18.96827783194638073, -5.556685674060065416, -8.875571351387176122 ) ) ;
#22598 = CARTESIAN_POINT ( 'NONE',  ( 24.36060779997411530, 9.641839768656376819, -1.940354640108606032 ) ) ;
#22599 = TOROIDAL_SURFACE ( 'NONE', #20298, 3.000000000000000000, 1.000000000000000000 ) ;
#22600 = CARTESIAN_POINT ( 'NONE',  ( 2.126485824405467628, 28.06267154637892247, -0.5579182477979972576 ) ) ;
#22601 = DIRECTION ( 'NONE',  ( 0.000000000000000000, -1.000000000000000000, 0.000000000000000000 ) ) ;
#22602 = ORIENTED_EDGE ( 'NONE', *, *, #4489, .F. ) ;
#22603 = CARTESIAN_POINT ( 'NONE',  ( 13.00000000000000000, -8.415881316778998311, -3.203269825092000200 ) ) ;
#22604 = CARTESIAN_POINT ( 'NONE',  ( 14.10412674931000154, -7.190271978224999749, -7.885398697387000944 ) ) ;
#22605 = CARTESIAN_POINT ( 'NONE',  ( -15.15688235000000006, 6.080933706674000128, -9.559848708078998669 ) ) ;
#22606 = DIRECTION ( 'NONE',  ( 0.9996848865506517967, 0.000000000000000000, 0.02510234256419879503 ) ) ;
#22607 = CARTESIAN_POINT ( 'NONE',  ( 16.14051537306000128, -10.16182289531000116, -3.745982005662999992 ) ) ;
#22608 = CARTESIAN_POINT ( 'NONE',  ( -12.41173981160000039, 6.613190111079999767, -13.46349570337000046 ) ) ;
#22609 = CARTESIAN_POINT ( 'NONE',  ( 0.000000000000000000, 21.50000000000000000, 0.000000000000000000 ) ) ;
#22610 = CARTESIAN_POINT ( 'NONE',  ( 23.94834967554000116, -9.057010814518001496, -3.671698204039999691 ) ) ;
#22611 = DIRECTION ( 'NONE',  ( 0.000000000000000000, 1.000000000000000000, 0.000000000000000000 ) ) ;
#22612 = ORIENTED_EDGE ( 'NONE', *, *, #19884, .T. ) ;
#22613 = DIRECTION ( 'NONE',  ( 0.000000000000000000, 0.000000000000000000, -1.000000000000000000 ) ) ;
#22614 = CARTESIAN_POINT ( 'NONE',  ( -1.595084814687000030, 26.58500240009999871, 2.387212940976999764 ) ) ;
#22615 = AXIS2_PLACEMENT_3D ( 'NONE', #12480, #1337, #10298 ) ;
#22616 = CARTESIAN_POINT ( 'NONE',  ( -2.670595826634000414, 11.74590557449999828, 4.055288669775002575 ) ) ;
#22617 = DIRECTION ( 'NONE',  ( -1.000000000000000000, 0.000000000000000000, 0.000000000000000000 ) ) ;
#22618 = CARTESIAN_POINT ( 'NONE',  ( -22.62446300055000137, -5.956939041310000071, -9.392211964618999431 ) ) ;
#22619 = ORIENTED_EDGE ( 'NONE', *, *, #1569, .F. ) ;
#22620 = FACE_OUTER_BOUND ( 'NONE', #22164, .T. ) ;
#22621 = ORIENTED_EDGE ( 'NONE', *, *, #12341, .F. ) ;
#22622 = CARTESIAN_POINT ( 'NONE',  ( -19.55887123173999953, -9.833822427806001798, 3.504477313184999776 ) ) ;
#22623 = CARTESIAN_POINT ( 'NONE',  ( -0.7160459369171999766, 28.54756359724000347, 2.361836001938000251 ) ) ;
#22624 = CYLINDRICAL_SURFACE ( 'NONE', #10361, 4.724999999999999645 ) ;
#22625 = CARTESIAN_POINT ( 'NONE',  ( 15.53006424931000140, -9.332187211223001100, 5.252733788881000621 ) ) ;
#22626 = CARTESIAN_POINT ( 'NONE',  ( -14.62071702128999995, 10.29594144910999809, -3.192455093500000007 ) ) ;
#22627 = CARTESIAN_POINT ( 'NONE',  ( 17.75418875731000057, 8.769310764750999354, 2.911614084577999861 ) ) ;
#22628 = CARTESIAN_POINT ( 'NONE',  ( 0.000000000000000000, 19.00000000000000000, 0.000000000000000000 ) ) ;
#22629 = ORIENTED_EDGE ( 'NONE', *, *, #13368, .F. ) ;
#22630 = FILL_AREA_STYLE_COLOUR ( '', #1505 ) ;
#22631 = CARTESIAN_POINT ( 'NONE',  ( 2.712095028381999562, 24.58106976543999878, -0.1465942787552000082 ) ) ;
#22632 = CARTESIAN_POINT ( 'NONE',  ( 13.85149880907578357, -8.793786893394734960, 5.371349140574870340 ) ) ;
#22633 = CARTESIAN_POINT ( 'NONE',  ( -0.8938142071318000426, 12.69387875947998978, -7.039327871081002996 ) ) ;
#22634 = CARTESIAN_POINT ( 'NONE',  ( 0.000000000000000000, 26.35000000000000142, 0.000000000000000000 ) ) ;
#22635 = CARTESIAN_POINT ( 'NONE',  ( -2.088906529886999763, 30.48427082063000171, -1.781945689819999901 ) ) ;
#22636 = CARTESIAN_POINT ( 'NONE',  ( 12.28022044530440660, 5.662962823301384674, 12.50000000000071410 ) ) ;
#22637 = CARTESIAN_POINT ( 'NONE',  ( 18.29495480302612620, 10.29737567282159105, -1.861358213112139337 ) ) ;
#22638 = CARTESIAN_POINT ( 'NONE',  ( 24.50000000000000000, -8.246372141814999779, 6.625187740483999832 ) ) ;
#22639 = FACE_OUTER_BOUND ( 'NONE', #4814, .T. ) ;
#22640 = ADVANCED_FACE ( 'NONE', ( #9126 ), #23409, .F. ) ;
#22641 = DIRECTION ( 'NONE',  ( 1.000000000000000000, 0.000000000000000000, 0.000000000000000000 ) ) ;
#22642 = ORIENTED_EDGE ( 'NONE', *, *, #646, .F. ) ;
#22643 = AXIS2_PLACEMENT_3D ( 'NONE', #12637, #21483, #19550 ) ;
#22644 = DIRECTION ( 'NONE',  ( -1.000000000000000000, 0.000000000000000000, 0.000000000000000000 ) ) ;
#22645 = EDGE_LOOP ( 'NONE', ( #2859, #19851, #13066, #6736 ) ) ;
#22646 = CARTESIAN_POINT ( 'NONE',  ( -5.534675601318385318, 16.14771134836236399, -2.628939291504586162 ) ) ;
#22648 = CARTESIAN_POINT ( 'NONE',  ( -0.8638410262558590125, 23.95255680022374989, 2.016069985583057722 ) ) ;
#22647 = DIRECTION ( 'NONE',  ( 1.000000000000000000, 0.000000000000000000, 0.000000000000000000 ) ) ;
#22649 = CARTESIAN_POINT ( 'NONE',  ( -0.3564538054804340383, 29.79977277844466954, -4.413003452969196161 ) ) ;
#22650 = ORIENTED_EDGE ( 'NONE', *, *, #5719, .F. ) ;
#22651 = CARTESIAN_POINT ( 'NONE',  ( 6.141065067267645894, 14.19649444987426179, -0.02421318643596113290 ) ) ;
#22652 = CARTESIAN_POINT ( 'NONE',  ( -6.086257062671249329, 16.07074762286712399, 1.021981042907482040 ) ) ;
#22653 = CARTESIAN_POINT ( 'NONE',  ( 0.000000000000000000, 29.84999999328000087, 0.000000000000000000 ) ) ;
#22654 = EDGE_CURVE ( 'NONE', #8639, #14252, #4027, .T. ) ;
#22655 = ORIENTED_EDGE ( 'NONE', *, *, #2067, .F. ) ;
#22656 = ORIENTED_EDGE ( 'NONE', *, *, #22219, .F. ) ;
#22657 = CARTESIAN_POINT ( 'NONE',  ( -14.00000000000000000, -3.369147568425823636, -9.111598281861018833 ) ) ;
#22658 = CARTESIAN_POINT ( 'NONE',  ( -12.13448613877000071, 13.17911648328999874, -7.610033336417999728 ) ) ;
#22659 = CARTESIAN_POINT ( 'NONE',  ( -0.1599369480228318985, 6.778540605024387489, -1.746824606910323707 ) ) ;
#22660 = FACE_OUTER_BOUND ( 'NONE', #4895, .T. ) ;
#22661 = ORIENTED_EDGE ( 'NONE', *, *, #20223, .F. ) ;
#22662 = CARTESIAN_POINT ( 'NONE',  ( -23.97728971651479313, 8.249343195704353704, 10.71120260265216118 ) ) ;
#22663 = AXIS2_PLACEMENT_3D ( 'NONE', #14274, #10162, #2897 ) ;
#22664 = DIRECTION ( 'NONE',  ( 0.000000000000000000, 0.000000000000000000, -1.000000000000000000 ) ) ;
#22665 = CARTESIAN_POINT ( 'NONE',  ( 15.54280282966749915, -5.820625934528824708, 8.599006677133495202 ) ) ;
#22666 = CIRCLE ( 'NONE', #7981, 7.200000000000000178 ) ;
#22667 = CARTESIAN_POINT ( 'NONE',  ( -15.99608434662999912, -10.91749873145000116, 1.679048479876000144 ) ) ;
#22668 = CARTESIAN_POINT ( 'NONE',  ( 0.3657816702587000091, 29.76730252947999844, -2.161985579530000035 ) ) ;
#22669 = CARTESIAN_POINT ( 'NONE',  ( -17.50529997408999705, -11.39253675243999986, 0.2566028257674999868 ) ) ;
#22670 = EDGE_CURVE ( 'NONE', #8412, #12128, #15160, .T. ) ;
#22671 = CARTESIAN_POINT ( 'NONE',  ( 0.4174375083360183369, 29.62843580719651015, 2.119604069544729796 ) ) ;
#22672 = ORIENTED_EDGE ( 'NONE', *, *, #16778, .T. ) ;
#22673 = VECTOR ( 'NONE', #9636, 1000.000000000000114 ) ;
#22674 = CARTESIAN_POINT ( 'NONE',  ( 2.091247443629999925, 24.02624597840999954, -0.6362363528857999384 ) ) ;
#22675 = DIRECTION ( 'NONE',  ( 1.351954405892998782E-08, -0.9999999999999990008, 4.357971159552991384E-08 ) ) ;
#22676 = ORIENTED_EDGE ( 'NONE', *, *, #6674, .T. ) ;
#22677 = CARTESIAN_POINT ( 'NONE',  ( -2.500000000000000000, 28.23419673618999681, 0.000000000000000000 ) ) ;
#22678 = CARTESIAN_POINT ( 'NONE',  ( -5.606396321587005183, 15.09360509207000867, 2.791161259578001541 ) ) ;
#22679 = CIRCLE ( 'NONE', #23076, 10.50000000000000000 ) ;
#22680 = CARTESIAN_POINT ( 'NONE',  ( -14.00000000000000000, -8.319952449050001420, 6.066771132503999020 ) ) ;
#22681 = EDGE_CURVE ( 'NONE', #19391, #5299, #18682, .T. ) ;
#22682 = CARTESIAN_POINT ( 'NONE',  ( 15.69656392131000011, 1.888996749216000026, -9.509257592937000680 ) ) ;
#22683 = ORIENTED_EDGE ( 'NONE', *, *, #15668, .F. ) ;
#22684 = DIRECTION ( 'NONE',  ( 0.000000000000000000, 1.000000000000000000, 0.000000000000000000 ) ) ;
#22685 = CARTESIAN_POINT ( 'NONE',  ( 24.32802197706137903, -12.60002805950083982, 3.176111224150924173 ) ) ;
#22686 = ORIENTED_EDGE ( 'NONE', *, *, #16370, .F. ) ;
#22687 = CARTESIAN_POINT ( 'NONE',  ( 0.000000000000000000, 19.04999994433000055, 0.000000000000000000 ) ) ;
#22688 = CARTESIAN_POINT ( 'NONE',  ( 11.92450592357447903, 8.469720391600080944, 10.33010329014251916 ) ) ;
#22689 = CARTESIAN_POINT ( 'NONE',  ( 4.347703729989003563, 12.46533150479998930, 1.901662359772999578 ) ) ;
#22690 = CARTESIAN_POINT ( 'NONE',  ( -14.00000000000000000, -1.433536925117362859, 9.728352550975314372 ) ) ;
#22691 = CARTESIAN_POINT ( 'NONE',  ( 18.05533209391456495, -1.235616904331040766, -10.33763051555462198 ) ) ;
#22692 = EDGE_CURVE ( 'NONE', #19340, #21630, #2408, .T. ) ;
#22693 = LINE ( 'NONE', #13495, #12938 ) ;
#22694 = DIRECTION ( 'NONE',  ( 0.9996708941621511579, -0.02565352539213875543, 0.000000000000000000 ) ) ;
#22695 = CARTESIAN_POINT ( 'NONE',  ( -6.637070260807000466, -19.10635214911999924, 2.000000000000000000 ) ) ;
#22696 = CARTESIAN_POINT ( 'NONE',  ( 6.162290176374000339, 13.65474020847999981, 2.204514988415999799 ) ) ;
#22697 = VECTOR ( 'NONE', #12291, 1000.000000000000000 ) ;
#22698 = CARTESIAN_POINT ( 'NONE',  ( -1.536366799937290084, 28.91753006952332328, -1.999167105995447669 ) ) ;
#22699 = CARTESIAN_POINT ( 'NONE',  ( -14.25243324638999809, -13.93375672974000068, 0.8660254037843999608 ) ) ;
#22700 = ADVANCED_FACE ( 'NONE', ( #11422 ), #18794, .T. ) ;
#22701 = CARTESIAN_POINT ( 'NONE',  ( -0.1032420033594618897, 30.39770183657784841, 2.157430679839748677 ) ) ;
#22702 = VERTEX_POINT ( 'NONE', #9477 ) ;
#22703 = EDGE_CURVE ( 'NONE', #21511, #21635, #7437, .T. ) ;
#22704 = CARTESIAN_POINT ( 'NONE',  ( -9.000000000000000000, 24.99999999999999645, -6.000000000000000000 ) ) ;
#22705 = CARTESIAN_POINT ( 'NONE',  ( -0.5951135560396972890, 12.81575860760598395, -6.640039254981911832 ) ) ;
#22706 = CARTESIAN_POINT ( 'NONE',  ( 1.182434930542719087, 29.94682129341587284, 3.936123028068912344 ) ) ;
#22707 = CARTESIAN_POINT ( 'NONE',  ( -20.75137991567049411, -4.596998218242912770, -9.457217556533679570 ) ) ;
#22708 = CARTESIAN_POINT ( 'NONE',  ( 2.291988582794999729, 27.18614211382000079, 0.04500887484482999495 ) ) ;
#22709 = CIRCLE ( 'NONE', #1844, 1.999999999999998668 ) ;
#22710 = CARTESIAN_POINT ( 'NONE',  ( -6.095789677045127419, 26.49783382847890678, 1.156958657242621147 ) ) ;
#22711 = ORIENTED_EDGE ( 'NONE', *, *, #6245, .F. ) ;
#22712 = CARTESIAN_POINT ( 'NONE',  ( -18.13094071507020288, 7.623672199478383149, 7.352634401449745560 ) ) ;
#22713 = EDGE_CURVE ( 'NONE', #1589, #14786, #9246, .T. ) ;
#22714 = DIRECTION ( 'NONE',  ( 0.7071067811905932254, 0.7071067811824932603, 1.099460927037990408E-07 ) ) ;
#22715 = EDGE_CURVE ( 'NONE', #13647, #15754, #5605, .T. ) ;
#22716 = CARTESIAN_POINT ( 'NONE',  ( -2.135272182958257492, 27.60654271691555905, -0.3931785795488860757 ) ) ;
#22717 = ORIENTED_EDGE ( 'NONE', *, *, #6601, .T. ) ;
#22718 = ORIENTED_EDGE ( 'NONE', *, *, #17430, .F. ) ;
#22719 = CARTESIAN_POINT ( 'NONE',  ( -18.76627150799833643, -8.263409740610351051, 4.078035658106594852 ) ) ;
#22720 = CARTESIAN_POINT ( 'NONE',  ( 16.51725174930999884, 10.44001970777000032, -2.498676648948999990 ) ) ;
#22721 = CARTESIAN_POINT ( 'NONE',  ( -13.19328898630000069, 9.449229977676001369, -4.943757532052999615 ) ) ;
#22722 = CARTESIAN_POINT ( 'NONE',  ( 0.000000000000000000, 21.50000000000000000, 0.000000000000000000 ) ) ;
#22723 = CARTESIAN_POINT ( 'NONE',  ( 16.95301537306000128, 10.84929791343999916, 0.2805791889531000227 ) ) ;
#22724 = CARTESIAN_POINT ( 'NONE',  ( 8.124934037954998800, -10.59999999999999964, 0.000000000000000000 ) ) ;
#22725 = CIRCLE ( 'NONE', #12693, 4.625000000000000000 ) ;
#22726 = DIRECTION ( 'NONE',  ( -0.000000000000000000, 1.000000000000000000, 0.000000000000000000 ) ) ;
#22727 = CARTESIAN_POINT ( 'NONE',  ( 22.43770138826000249, 7.394962502173999752, -7.113329243426999682 ) ) ;
#22728 = CARTESIAN_POINT ( 'NONE',  ( 4.000000000000058620, 24.75094615492120553, -2.107036910272262364 ) ) ;
#22729 = ORIENTED_EDGE ( 'NONE', *, *, #3738, .T. ) ;
#22730 = CARTESIAN_POINT ( 'NONE',  ( 11.87172645921999958, -2.663994189788999822, -8.934245366879000727 ) ) ;
#22731 = CARTESIAN_POINT ( 'NONE',  ( -0.3657850755361999884, 28.13706776952000155, 2.644546391786999795 ) ) ;
#22732 = CARTESIAN_POINT ( 'NONE',  ( 3.971078888290999309, 12.18367478550000982, 2.673022683980000647 ) ) ;
#22733 = CARTESIAN_POINT ( 'NONE',  ( 2.158192071364979370, 28.99867104832394560, 0.08873628542675822406 ) ) ;
#22734 = CONICAL_SURFACE ( 'NONE', #21215, 13.23032192316000000, 1.093540295016705466 ) ;
#22735 = CARTESIAN_POINT ( 'NONE',  ( -21.12070208853000253, -11.05482043179000051, 0.7640197540441000523 ) ) ;
#22736 = ORIENTED_EDGE ( 'NONE', *, *, #13547, .F. ) ;
#22737 = CARTESIAN_POINT ( 'NONE',  ( -9.000000000000000000, 24.99999999999999645, 1.000000000000000000 ) ) ;
#22738 = VECTOR ( 'NONE', #3650, 1000.000000000000000 ) ;
#22739 = ORIENTED_EDGE ( 'NONE', *, *, #12210, .F. ) ;
#22740 = CARTESIAN_POINT ( 'NONE',  ( 0.000000000000000000, 30.00000000000000000, 0.000000000000000000 ) ) ;
#22741 = ADVANCED_FACE ( 'NONE', ( #18570 ), #3793, .T. ) ;
#22742 = CARTESIAN_POINT ( 'NONE',  ( 3.799035759646001154, 13.17963623137001505, 5.991547988457999629 ) ) ;
#22743 = CONICAL_SURFACE ( 'NONE', #1879, 4.649999883068000273, 0.7853981633972997312 ) ;
#22744 = CARTESIAN_POINT ( 'NONE',  ( -12.25000000000000000, 15.45000000000000107, 0.000000000000000000 ) ) ;
#22745 = CARTESIAN_POINT ( 'NONE',  ( 15.96881424931000026, -5.728615299830999597, -9.061514726575000012 ) ) ;
#22746 = CARTESIAN_POINT ( 'NONE',  ( -17.66767224083000087, -1.527991571549000005, 10.75645198264999891 ) ) ;
#22747 = CARTESIAN_POINT ( 'NONE',  ( 17.42512625730999787, 6.303186173173999762, -6.744507379544999459 ) ) ;
#22748 = CARTESIAN_POINT ( 'NONE',  ( 24.36414987671881960, 12.39811243366166416, -3.525839346946420427 ) ) ;
#22749 = VECTOR ( 'NONE', #15369, 1000.000000000000000 ) ;
#22750 = ORIENTED_EDGE ( 'NONE', *, *, #10633, .F. ) ;
#22751 = CARTESIAN_POINT ( 'NONE',  ( 12.51793201921000076, -13.93375672974000068, -0.7216659839314999436 ) ) ;
#22752 = CARTESIAN_POINT ( 'NONE',  ( -2.709454201502000004, 24.96531645185000059, -0.1892281976294000190 ) ) ;
#22753 = CARTESIAN_POINT ( 'NONE',  ( 14.06984511579193331, -10.11168233347247813, -2.157631914311957999 ) ) ;
#22754 = AXIS2_PLACEMENT_3D ( 'NONE', #4174, #15296, #6345 ) ;
#22755 = CARTESIAN_POINT ( 'NONE',  ( 2.838808265031001810, 14.18773367037002409, -5.481123045573999875 ) ) ;
#22756 = DIRECTION ( 'NONE',  ( 2.979867880226000256E-10, 9.527955641186100052E-24, -1.000000000000000000 ) ) ;
#22757 = CARTESIAN_POINT ( 'NONE',  ( 0.000000000000000000, 18.50000000000000000, 0.000000000000000000 ) ) ;
#22758 = CARTESIAN_POINT ( 'NONE',  ( 11.18529249867571984, -1.746922494864825426, 12.50002083036580913 ) ) ;
#22759 = CARTESIAN_POINT ( 'NONE',  ( 17.73741084492538889, -5.461382820680055872, -9.083679806854396688 ) ) ;
#22760 = DIRECTION ( 'NONE',  ( 1.000000000000000000, 0.000000000000000000, 0.000000000000000000 ) ) ;
#22761 = AXIS2_PLACEMENT_3D ( 'NONE', #6948, #21730, #12524 ) ;
#22762 = CARTESIAN_POINT ( 'NONE',  ( 0.000000000000000000, -7.216878364870000340, 12.50000000000000000 ) ) ;
#22763 = CARTESIAN_POINT ( 'NONE',  ( -6.046837210729000489, 16.30334039894000142, -1.000000000000000000 ) ) ;
#22764 = VERTEX_POINT ( 'NONE', #22308 ) ;
#22765 = CARTESIAN_POINT ( 'NONE',  ( 0.5500000000000000444, 1.217911241751999838E-14, 0.000000000000000000 ) ) ;
#22766 = EDGE_LOOP ( 'NONE', ( #16489, #3600, #21519, #19109 ) ) ;
#22767 = CIRCLE ( 'NONE', #10033, 4.750000000000000000 ) ;
#22768 = DIRECTION ( 'NONE',  ( 0.000000000000000000, 0.000000000000000000, -1.000000000000000000 ) ) ;
#22770 = CARTESIAN_POINT ( 'NONE',  ( 4.749999673578000348, 12.55004296393999930, -4.341645649670000483E-06 ) ) ;
#22769 = CARTESIAN_POINT ( 'NONE',  ( -2.351879151723880845, 11.71687587877330117, 4.209509496448244015 ) ) ;
#22771 = CARTESIAN_POINT ( 'NONE',  ( 24.12867869089190265, -9.461899957204449763, 0.6956614285005767728 ) ) ;
#22772 = CARTESIAN_POINT ( 'NONE',  ( -20.51955273722667172, -2.691069519324763348, 8.860573964823370119 ) ) ;
#22773 = CARTESIAN_POINT ( 'NONE',  ( 23.99062354302999722, -6.216878364870000340, -12.50000000000000000 ) ) ;
#22774 = VERTEX_POINT ( 'NONE', #9596 ) ;
#22775 = VERTEX_POINT ( 'NONE', #13111 ) ;
#22776 = DIRECTION ( 'NONE',  ( -0.9999999999810907925, 6.097499773276291543E-06, 7.994200222768927623E-07 ) ) ;
#22777 = CIRCLE ( 'NONE', #21245, 5.000000000000004441 ) ;
#22778 = CARTESIAN_POINT ( 'NONE',  ( -0.1529142988638288181, 26.50000000000000355, -2.395123632968240823 ) ) ;
#22779 = CARTESIAN_POINT ( 'NONE',  ( -14.25243324638999809, -7.716878364870000340, -11.63397459621999985 ) ) ;
#22780 = ADVANCED_FACE ( 'NONE', ( #20507 ), #18447, .T. ) ;
#22781 = ORIENTED_EDGE ( 'NONE', *, *, #79, .F. ) ;
#22782 = CARTESIAN_POINT ( 'NONE',  ( -21.14497945657000244, 8.262325765017999757, 5.001268951993999679 ) ) ;
#22783 = CARTESIAN_POINT ( 'NONE',  ( 1.724048102327889520, 12.96513651749977214, -1.060396748501814868 ) ) ;
#22784 = CARTESIAN_POINT ( 'NONE',  ( 6.157064176825728374, 14.08830590709009556, 0.3628796317935392146 ) ) ;
#22785 = CARTESIAN_POINT ( 'NONE',  ( 15.28176760385781385, 3.108477508404123846, 9.870308429438537701 ) ) ;
#22786 = CARTESIAN_POINT ( 'NONE',  ( -17.98338081197000093, -8.100370408748000628, 7.589501626130000567 ) ) ;
#22787 = CIRCLE ( 'NONE', #11211, 9.030549305585997999 ) ;
#22788 = CARTESIAN_POINT ( 'NONE',  ( 1.660950793280000060, 28.72156950879999826, 1.671267114093999862 ) ) ;
#22789 = CARTESIAN_POINT ( 'NONE',  ( -21.46225067249296359, -8.457439661898087380, 6.476282215921202123 ) ) ;
#22790 = AXIS2_PLACEMENT_3D ( 'NONE', #17903, #21658, #12454 ) ;
#22791 = CARTESIAN_POINT ( 'NONE',  ( -16.24575980504999606, 10.15426072268999924, 3.750674035441000420 ) ) ;
#22792 = EDGE_CURVE ( 'NONE', #13433, #9495, #2811, .T. ) ;
#22793 = CARTESIAN_POINT ( 'NONE',  ( -0.8197724292390062839, 29.55421540811686398, 2.000496916279093540 ) ) ;
#22794 = ORIENTED_EDGE ( 'NONE', *, *, #8672, .T. ) ;
#22795 = CARTESIAN_POINT ( 'NONE',  ( -0.07403871084495999844, 24.61795039184000089, 2.347720816621999607 ) ) ;
#22796 = CARTESIAN_POINT ( 'NONE',  ( -18.63025570457361013, 10.07612922007779765, -2.841683973627437076 ) ) ;
#22797 = ORIENTED_EDGE ( 'NONE', *, *, #5517, .F. ) ;
#22798 = CARTESIAN_POINT ( 'NONE',  ( 5.975665869958996623, 14.53417513656000182, -1.387968629032001910 ) ) ;
#22799 = CARTESIAN_POINT ( 'NONE',  ( -2.500000000000000000, 26.63419673618999894, 0.000000000000000000 ) ) ;
#22800 = CARTESIAN_POINT ( 'NONE',  ( -20.44776253787999920, -9.196011600180998613, 0.000000000000000000 ) ) ;
#22801 = CARTESIAN_POINT ( 'NONE',  ( 15.91593892131000132, 7.924234377949000319, -5.595770532261999719 ) ) ;
#22802 = ORIENTED_EDGE ( 'NONE', *, *, #18262, .T. ) ;
#22803 = DIRECTION ( 'NONE',  ( 1.000000000000000000, 0.000000000000000000, 0.000000000000000000 ) ) ;
#22804 = DIRECTION ( 'NONE',  ( -0.000000000000000000, 1.000000000000000000, 0.000000000000000000 ) ) ;
#22805 = CARTESIAN_POINT ( 'NONE',  ( 24.50000000000000000, -10.82531754731000007, 6.250000000000000000 ) ) ;
#22806 = EDGE_CURVE ( 'NONE', #15568, #959, #19073, .T. ) ;
#22807 = VERTEX_POINT ( 'NONE', #8386 ) ;
#22808 = CARTESIAN_POINT ( 'NONE',  ( 4.000000000000000000, 26.31534065533125144, -1.802053058880663805 ) ) ;
#22809 = DIRECTION ( 'NONE',  ( 1.000000000000000000, 0.000000000000000000, 2.088600023070000287E-09 ) ) ;
#22810 = CARTESIAN_POINT ( 'NONE',  ( 24.08830182848186041, 5.395025589383775078, 9.150520802871518811 ) ) ;
#22811 = CARTESIAN_POINT ( 'NONE',  ( 1.709999999999999964, 9.852710287022999225, -7.500000000000000000 ) ) ;
#22812 = CARTESIAN_POINT ( 'NONE',  ( 18.19747459623542341, 3.794755501146056975, -9.726389436706863734 ) ) ;
#22813 = AXIS2_PLACEMENT_3D ( 'NONE', #3830, #7939, #417 ) ;
#22814 = CARTESIAN_POINT ( 'NONE',  ( 12.00000000000000000, -9.140869530236654938, -4.136866240621976054 ) ) ;
#22815 = LINE ( 'NONE', #6105, #5658 ) ;
#22816 = CARTESIAN_POINT ( 'NONE',  ( -3.412554491691996539, 13.99161680779000605, -5.089445285121002804 ) ) ;
#22817 = CARTESIAN_POINT ( 'NONE',  ( 0.000000000000000000, 7.100000000000000533, 0.000000000000000000 ) ) ;
#22818 = B_SPLINE_CURVE_WITH_KNOTS ( 'NONE', 3,
 ( #13762, #11967, #21164, #15460, #8327, #4575, #22845, #23083, #19356, #21294, #6258, #3007, #2883, #10266, #1183, #10392, #17654, #1053, #8454, #15821, #23212, #14017, #21407, #18254, #18146, #21657, #5415, #5070, #7339, #3249, #3135, #22117, #1423, #12800, #14607, #12903, #20074, #18363, #1549, #20187, #10635, #7102, #16058, #8935, #16539, #23930, #6989, #3597, #22002, #12453, #14720, #19836, #3489, #10751, #5524, #18022, #10980, #10519, #16182, #16303, #1775, #17902, #8694, #21884, #1305, #12566, #5184, #1656, #9162, #23453, #8823, #19954, #6867, #14259, #12686, #23585, #23694, #14378, #10869, #21772, #14492, #3373, #5295, #9045, #16417, #23807 ),
 .UNSPECIFIED., .F., .F.,
 ( 4, 2, 1, 2, 2, 2, 2, 2, 2, 1, 2, 2, 2, 2, 2, 2, 1, 2, 2, 2, 2, 2, 2, 2, 2, 1, 2, 2, 2, 2, 2, 2, 1, 2, 2, 2, 2, 2, 2, 2, 1, 2, 2, 2, 2, 4 ),
 ( 0.000000000000000000, 0.01325029465915758195, 0.02650058931831516390, 0.03975088397747275626, 0.05300117863663034862, 0.07950176795494552640, 0.1060023572732606972, 0.1325029465915758820, 0.1457532412507334951, 0.1590035359098910805, 0.1722538305690486660, 0.1855041252282062791, 0.2120047145465215055, 0.2385053038648367041, 0.2650058931831518749, 0.2782561878423095436, 0.2915064825014671568, 0.3047567771606247700, 0.3180070718197824386, 0.3312573664789400518, 0.3445076611380976095, 0.3710082504564127803, 0.3975088397747280067, 0.4240094290930431775, 0.4372597237522007907, 0.4505100184113584039, 0.4637603130705159060, 0.4770106077296734637, 0.5035111970479886345, 0.5300117863663037499, 0.5565123756846189762, 0.5697626703437765894, 0.5830129650029342026, 0.5962632596620918157, 0.6095135543212493179, 0.6360141436395645442, 0.6625147329578798816, 0.6890153222761951080, 0.7155159115945103343, 0.7287662062536679475, 0.7420165009128254496, 0.7552667955719830628, 0.7685170902311406760, 0.7950176795494559023, 0.8215182688677710177, 0.8480188581860863550 ),
 .UNSPECIFIED. ) ;
#22819 = CARTESIAN_POINT ( 'NONE',  ( 0.7318187998270080374, 26.37490599056236817, -4.196286372439437251 ) ) ;
#22820 = CARTESIAN_POINT ( 'NONE',  ( 0.000000000000000000, 21.89999999999999858, 0.000000000000000000 ) ) ;
#22821 = EDGE_CURVE ( 'NONE', #16017, #16978, #1759, .T. ) ;
#22822 = CARTESIAN_POINT ( 'NONE',  ( -0.3725721029586212540, 30.38186967353806978, 2.129277066162170939 ) ) ;
#22823 = ORIENTED_EDGE ( 'NONE', *, *, #13261, .T. ) ;
#22824 = CARTESIAN_POINT ( 'NONE',  ( 20.66608820303999750, -8.164859526374000254, 7.177460020925999551 ) ) ;
#22825 = CARTESIAN_POINT ( 'NONE',  ( -3.554379017154496445, 13.22735737994497462, -5.777226003025122125 ) ) ;
#22826 = CARTESIAN_POINT ( 'NONE',  ( 0.3564538054804340383, 29.79977277844466954, 4.413003452969196161 ) ) ;
#22827 = CARTESIAN_POINT ( 'NONE',  ( -19.62677216480515696, -3.112713671263979354, 10.01251316358262144 ) ) ;
#22828 = CARTESIAN_POINT ( 'NONE',  ( 0.1349572241792000027, 27.38114211381999752, -2.288454502553999959 ) ) ;
#22829 = CARTESIAN_POINT ( 'NONE',  ( 60.61494135913342518, 35.51856778792605240, 0.000000000000000000 ) ) ;
#22830 = ORIENTED_EDGE ( 'NONE', *, *, #10234, .F. ) ;
#22831 = EDGE_CURVE ( 'NONE', #10425, #5775, #3586, .T. ) ;
#22832 = CARTESIAN_POINT ( 'NONE',  ( -17.12613617482062267, -4.646914316943434820, -9.333643767870253072 ) ) ;
#22833 = CARTESIAN_POINT ( 'NONE',  ( -4.000000000000000000, 29.93562577624027554, -1.040161751118715117 ) ) ;
#22834 = CARTESIAN_POINT ( 'NONE',  ( 0.000000000000000000, 7.216878364870000340, -12.50000000000000000 ) ) ;
#22835 = AXIS2_PLACEMENT_3D ( 'NONE', #22740, #456, #10164 ) ;
#22836 = DIRECTION ( 'NONE',  ( -1.000000000000000000, 0.000000000000000000, 0.000000000000000000 ) ) ;
#22837 = EDGE_CURVE ( 'NONE', #5348, #11953, #16331, .T. ) ;
#22838 = ORIENTED_EDGE ( 'NONE', *, *, #4955, .T. ) ;
#22839 = DIRECTION ( 'NONE',  ( 0.000000000000000000, 0.9512662730843030046, -0.3083706822840010520 ) ) ;
#22840 = CARTESIAN_POINT ( 'NONE',  ( 17.72381424930999927, -7.480404092888999656, -7.743571870822999692 ) ) ;
#22841 = CARTESIAN_POINT ( 'NONE',  ( -14.00000000000000000, 6.995278287856000254, -5.711120943918999160 ) ) ;
#22842 = CARTESIAN_POINT ( 'NONE',  ( -17.79757687361000151, -8.527194750238999532, 7.571551323727999439 ) ) ;
#22843 = CARTESIAN_POINT ( 'NONE',  ( 23.92506969171387965, -8.172088213226873066, -4.569912402413578434 ) ) ;
#22844 = CARTESIAN_POINT ( 'NONE',  ( 18.84931994526000310, 8.383432096882000195, -6.096962826690000448 ) ) ;
#22845 = CARTESIAN_POINT ( 'NONE',  ( -1.874306020383145643, 28.67199880806925094, 1.099966823684755957 ) ) ;
#22846 = CARTESIAN_POINT ( 'NONE',  ( -12.06624327026009347, 1.368548241523999952E-14, 0.000000000000000000 ) ) ;
#22847 = CARTESIAN_POINT ( 'NONE',  ( 21.02130857102000050, 8.371468613062001296, 5.866070922022999845 ) ) ;
#22848 = EDGE_CURVE ( 'NONE', #22108, #23527, #10323, .T. ) ;
#22849 = CARTESIAN_POINT ( 'NONE',  ( 3.145406728938545893, 29.89685207198635553, 2.802800731853388960 ) ) ;
#22850 = ORIENTED_EDGE ( 'NONE', *, *, #21996, .F. ) ;
#22851 = CARTESIAN_POINT ( 'NONE',  ( -3.000000000000000000, 17.89999999999999858, 0.000000000000000000 ) ) ;
#22852 = CARTESIAN_POINT ( 'NONE',  ( 2.219793368323999871, 28.42956776951999842, -1.483218624018999954 ) ) ;
#22853 = B_SPLINE_CURVE_WITH_KNOTS ( 'NONE', 3,
 ( #12147, #14073, #21468, #19409, #19892, #15757, #19657, #2823, #10456, #1485, #23147, #3308, #6568, #13952, #17845, #21346, #23385, #12396 ),
 .UNSPECIFIED., .F., .F.,
 ( 4, 2, 2, 2, 2, 2, 2, 2, 4 ),
 ( 0.000000000000000000, 0.1250000000000000000, 0.2500000000000000000, 0.3750000000000000000, 0.5000000000000000000, 0.6250000000000000000, 0.7500000000000000000, 0.8750000000000000000, 1.000000000000000000 ),
 .UNSPECIFIED. ) ;
#22854 = CARTESIAN_POINT ( 'NONE',  ( 3.310881862312000656, 11.97843584064001199, 3.462059838974000936 ) ) ;
#22855 = CARTESIAN_POINT ( 'NONE',  ( 2.156475325630220485, 28.99669585034901331, 0.1219500803027313146 ) ) ;
#22856 = CARTESIAN_POINT ( 'NONE',  ( -20.28527935963000317, 10.50778539144999968, -3.446350770996999824 ) ) ;
#22857 = ORIENTED_EDGE ( 'NONE', *, *, #3336, .F. ) ;
#22858 = CARTESIAN_POINT ( 'NONE',  ( -6.406610618360471854, 27.98165854022565213, 0.9999999999999870104 ) ) ;
#22859 = ORIENTED_EDGE ( 'NONE', *, *, #19768, .F. ) ;
#22860 = CARTESIAN_POINT ( 'NONE',  ( 15.25783103379665384, -5.569620820083297730, -7.247153067674876326 ) ) ;
#22861 = CARTESIAN_POINT ( 'NONE',  ( -4.000000000000000000, 26.50000000000000355, 0.000000000000000000 ) ) ;
#22862 = CARTESIAN_POINT ( 'NONE',  ( -1.703378280910000875, 12.85045892059999595, 6.244730413338999142 ) ) ;
#22863 = CARTESIAN_POINT ( 'NONE',  ( -0.6074916215089999350, 30.83999999999999986, -2.072813047478000215 ) ) ;
#22864 = CARTESIAN_POINT ( 'NONE',  ( -14.25546320177999959, 6.466449120341000167, 12.35591025714999880 ) ) ;
#22865 = EDGE_CURVE ( 'NONE', #21237, #11791, #15944, .T. ) ;
#22866 = EDGE_CURVE ( 'NONE', #17884, #3424, #20385, .T. ) ;
#22867 = CARTESIAN_POINT ( 'NONE',  ( -15.02697771723000031, -1.474210749020000044, -10.68967233462999999 ) ) ;
#22868 = CARTESIAN_POINT ( 'NONE',  ( 17.53481375730999758, 8.357543471651000644, -3.927243979254000372 ) ) ;
#22869 = CARTESIAN_POINT ( 'NONE',  ( 1.536366799937295413, 27.48333333333333073, 1.999167105995444338 ) ) ;
#22870 = ORIENTED_EDGE ( 'NONE', *, *, #3583, .T. ) ;
#22871 = CARTESIAN_POINT ( 'NONE',  ( 19.70552847921732464, -0.05221305801487967357, -10.50537839887272185 ) ) ;
#22872 = CARTESIAN_POINT ( 'NONE',  ( 1.937464785723999938, 25.39095665442000183, 1.620130890068999907 ) ) ;
#22873 = CARTESIAN_POINT ( 'NONE',  ( 13.52121136864142414, 1.289066941492836849, 10.24442406412049067 ) ) ;
#22874 = ORIENTED_EDGE ( 'NONE', *, *, #11622, .T. ) ;
#22875 = CARTESIAN_POINT ( 'NONE',  ( 4.878371034287997787, 14.94155586047998874, -3.715635765802999035 ) ) ;
#22876 = DIRECTION ( 'NONE',  ( 0.000000000000000000, -0.8660254037844288266, -0.5000000000000169864 ) ) ;
#22877 = CARTESIAN_POINT ( 'NONE',  ( 1.699999999999999956, 13.00000000000000000, 1.053565375285000050 ) ) ;
#22878 = EDGE_CURVE ( 'NONE', #14280, #21303, #6670, .T. ) ;
#22879 = CARTESIAN_POINT ( 'NONE',  ( 14.70899999999999963, -9.048743642952000954, 0.000000000000000000 ) ) ;
#22880 = ADVANCED_FACE ( 'NONE', ( #8017 ), #17466, .F. ) ;
#22881 = DIRECTION ( 'NONE',  ( -0.000000000000000000, 0.6324223201336057754, 0.7746237854577066040 ) ) ;
#22882 = FACE_OUTER_BOUND ( 'NONE', #16046, .T. ) ;
#22883 = FACE_OUTER_BOUND ( 'NONE', #16472, .T. ) ;
#22884 = CARTESIAN_POINT ( 'NONE',  ( -1.999167105995453442, 29.75086340285666253, -1.536366799937283645 ) ) ;
#22885 = ORIENTED_EDGE ( 'NONE', *, *, #7884, .F. ) ;
#22886 = CARTESIAN_POINT ( 'NONE',  ( 11.45478115326693747, -12.39608915220626528, 3.529209591781598654 ) ) ;
#22887 = ORIENTED_EDGE ( 'NONE', *, *, #11575, .F. ) ;
#22888 = CARTESIAN_POINT ( 'NONE',  ( 12.00000000000000000, -9.392874664203999302, -3.575135015595999999 ) ) ;
#22890 = CARTESIAN_POINT ( 'NONE',  ( 1.626223296995356726, 24.10999786935245837, 1.471899765573001506 ) ) ;
#22889 = CARTESIAN_POINT ( 'NONE',  ( -2.884120348847549309, 11.83272722737032190, 3.874092213913487015 ) ) ;
#22891 = CARTESIAN_POINT ( 'NONE',  ( -3.224906711384808666, 13.15387152289895134, 5.942239841201511830 ) ) ;
#22892 = CIRCLE ( 'NONE', #3962, 10.69999999999999929 ) ;
#22893 = CARTESIAN_POINT ( 'NONE',  ( 16.93748565861000088, 10.60378489164999927, 3.221716779813999842 ) ) ;
#22894 = CARTESIAN_POINT ( 'NONE',  ( 0.000000000000000000, 17.95000004008999994, 0.000000000000000000 ) ) ;
#22895 = CARTESIAN_POINT ( 'NONE',  ( -2.183184479328999839, 26.48419433609999984, -1.864615697012000028 ) ) ;
#22896 = VERTEX_POINT ( 'NONE', #860 ) ;
#22897 = ORIENTED_EDGE ( 'NONE', *, *, #7317, .F. ) ;
#22898 = CARTESIAN_POINT ( 'NONE',  ( -14.00000000000000178, -7.049815569282562144, -6.985318574217756371 ) ) ;
#22899 = CARTESIAN_POINT ( 'NONE',  ( -0.5801485360015447013, 6.802422194044264181, -1.651406016847994263 ) ) ;
#22900 = FACE_OUTER_BOUND ( 'NONE', #22766, .T. ) ;
#22901 = ORIENTED_EDGE ( 'NONE', *, *, #17675, .T. ) ;
#22902 = CARTESIAN_POINT ( 'NONE',  ( -18.74584515806999718, -8.073393492905999835, 5.180320272283000627 ) ) ;
#22903 = CARTESIAN_POINT ( 'NONE',  ( -2.000000000000000000, 31.00000000000000000, 0.000000000000000000 ) ) ;
#22904 = CARTESIAN_POINT ( 'NONE',  ( 6.225701887381084987, 13.76125012799850467, 1.306893872209164753 ) ) ;
#22905 = CARTESIAN_POINT ( 'NONE',  ( 15.66748608625431416, -8.878148344715427243, 5.320606095657832491 ) ) ;
#22906 = CARTESIAN_POINT ( 'NONE',  ( -18.88669738713000257, 8.214810501480998894, -7.502223699012001035 ) ) ;
#22907 = CARTESIAN_POINT ( 'NONE',  ( 4.834779662050625149, 12.44818287292682335, -0.2493690240449278894 ) ) ;
#22908 = CARTESIAN_POINT ( 'NONE',  ( -20.07255388211770963, 5.526680004444125771, 8.922835914469294138 ) ) ;
#22909 = AXIS2_PLACEMENT_3D ( 'NONE', #22166, #12957, #20355 ) ;
#22910 = CARTESIAN_POINT ( 'NONE',  ( -14.86460545047999915, 10.81390249068999942, -3.353128725732000159 ) ) ;
#22911 = CARTESIAN_POINT ( 'NONE',  ( -1.517536029622082783, 29.50471637792290025, 1.536878451077771768 ) ) ;
#22912 = EDGE_LOOP ( 'NONE', ( #9982, #8953, #7254 ) ) ;
#22913 = CARTESIAN_POINT ( 'NONE',  ( 2.247188694785000163, 24.05956826785000047, -0.6836795634928000132 ) ) ;
#22914 = CARTESIAN_POINT ( 'NONE',  ( -14.54983219195056243, 2.782516519562602930, 9.977023446843118037 ) ) ;
#22915 = ORIENTED_EDGE ( 'NONE', *, *, #17321, .F. ) ;
#22916 = CARTESIAN_POINT ( 'NONE',  ( -3.574282176492461098E-06, 28.76916452463145291, 2.098900968869932715 ) ) ;
#22917 = CARTESIAN_POINT ( 'NONE',  ( 5.365624983119998248, 14.28158000389998783, -2.870197123060997502 ) ) ;
#22918 = CARTESIAN_POINT ( 'NONE',  ( -2.141135906240991371, 30.84841738671447331, 0.2119206051068452390 ) ) ;
#22919 = CARTESIAN_POINT ( 'NONE',  ( -20.06984587121332808, -2.404380842926237882, -8.947266942397744671 ) ) ;
#22920 = CARTESIAN_POINT ( 'NONE',  ( 11.56500142131000075, -9.431037050546001055, -0.2079650321152999859 ) ) ;
#22921 = ORIENTED_EDGE ( 'NONE', *, *, #12669, .F. ) ;
#22922 = AXIS2_PLACEMENT_3D ( 'NONE', #13306, #3885, #7503 ) ;
#22923 = FACE_OUTER_BOUND ( 'NONE', #7556, .T. ) ;
#22924 = CARTESIAN_POINT ( 'NONE',  ( -1.259047450927251566, 27.06666666666667354, -2.184465970885643316 ) ) ;
#22925 = DIRECTION ( 'NONE',  ( -1.000000000000000000, 0.000000000000000000, 0.000000000000000000 ) ) ;
#22926 = PRODUCT ( 'MAS-673', 'MAS-673', '', ( #19345 ) ) ;
#22927 = VERTEX_POINT ( 'NONE', #15390 ) ;
#22928 = DIRECTION ( 'NONE',  ( -1.000000000000000000, 0.000000000000000000, 0.000000000000000000 ) ) ;
#22929 = CARTESIAN_POINT ( 'NONE',  ( 11.78693030655652763, 8.669062849316338415, 9.984739426213851132 ) ) ;
#22930 = DIRECTION ( 'NONE',  ( -1.000000000000000000, 0.000000000000000000, 0.000000000000000000 ) ) ;
#22931 = CARTESIAN_POINT ( 'NONE',  ( -8.099999999999999645, 10.59999999999999964, 4.735458969396000849E-10 ) ) ;
#22932 = CARTESIAN_POINT ( 'NONE',  ( 18.38725600494685963, 8.888177610145580942, -5.441499180344855802 ) ) ;
#22933 = CARTESIAN_POINT ( 'NONE',  ( -14.00000000000000000, 1.396097351027999937E-14, 0.000000000000000000 ) ) ;
#22934 = B_SPLINE_CURVE_WITH_KNOTS ( 'NONE', 3,
 ( #4089, #13525, #10028, #22843, #9659, #2505 ),
 .UNSPECIFIED., .F., .F.,
 ( 4, 2, 4 ),
 ( 0.8039802372034564604, 0.9019901186017282857, 1.000000000000000000 ),
 .UNSPECIFIED. ) ;
#22935 = CARTESIAN_POINT ( 'NONE',  ( -14.39391672138606637, 12.88860090843610351, -2.676267392864989603 ) ) ;
#22936 = CARTESIAN_POINT ( 'NONE',  ( 19.53721867119999800, -1.916595458125999851, -11.01322041192999990 ) ) ;
#22937 = CARTESIAN_POINT ( 'NONE',  ( -11.00000000000000000, 10.59999999999999964, 0.000000000000000000 ) ) ;
#22938 = CARTESIAN_POINT ( 'NONE',  ( -3.755314868451799626, 14.14753470886829234, -4.866744050934065591 ) ) ;
#22939 = CARTESIAN_POINT ( 'NONE',  ( -6.099196000000000062, 16.31160201366999729, -2.000000000000000000 ) ) ;
#22940 = CARTESIAN_POINT ( 'NONE',  ( -0.7323698196505201707, 30.04763029221750514, -2.036741068021854506 ) ) ;
#22941 = ORIENTED_EDGE ( 'NONE', *, *, #12487, .T. ) ;
#22942 = CARTESIAN_POINT ( 'NONE',  ( 20.61352647260000026, -10.32027106859000121, 0.5347350817453000449 ) ) ;
#22943 = CARTESIAN_POINT ( 'NONE',  ( -3.062204858405229047, 13.12005258919790407, -6.016671387275827954 ) ) ;
#22944 = CARTESIAN_POINT ( 'NONE',  ( -1.177500171710576859, 23.61738672577268972, -1.759779639892373959 ) ) ;
#22945 = EDGE_CURVE ( 'NONE', #15263, #1761, #12098, .T. ) ;
#22946 = CARTESIAN_POINT ( 'NONE',  ( -19.46611391468236008, -7.928063235344735560, 6.854333141353487591 ) ) ;
#22947 = LINE ( 'NONE', #8560, #1141 ) ;
#22948 = AXIS2_PLACEMENT_3D ( 'NONE', #6343, #9861, #13726 ) ;
#22949 = CARTESIAN_POINT ( 'NONE',  ( 0.3815877974581001753, 11.45498001497000118, -4.936402010209000046 ) ) ;
#22950 = EDGE_LOOP ( 'NONE', ( #21388, #6705, #1829, #1728 ) ) ;
#22951 = CARTESIAN_POINT ( 'NONE',  ( -16.84702380252937459, 5.079908938365492510, -9.198943836403035590 ) ) ;
#22952 = CARTESIAN_POINT ( 'NONE',  ( -1.989999999999999991, 13.00000000000000000, 7.500000000000000000 ) ) ;
#22953 = LINE ( 'NONE', #2496, #15231 ) ;
#22954 = CARTESIAN_POINT ( 'NONE',  ( 0.000000000000000000, 23.00000000000000000, 0.000000000000000000 ) ) ;
#22955 = EDGE_CURVE ( 'NONE', #14560, #3493, #20676, .T. ) ;
#22956 = ORIENTED_EDGE ( 'NONE', *, *, #333, .F. ) ;
#22957 = CARTESIAN_POINT ( 'NONE',  ( 4.000000000000000000, 30.00000000000000000, 0.000000000000000000 ) ) ;
#22958 = CARTESIAN_POINT ( 'NONE',  ( 13.22662674931000204, 6.334720884006999952, 8.559150566242998082 ) ) ;
#22959 = CIRCLE ( 'NONE', #22192, 15.45000000000000107 ) ;
#22960 = CARTESIAN_POINT ( 'NONE',  ( -21.65013772846999984, -0.7453069750031999785, 11.13564762747999914 ) ) ;
#22961 = CARTESIAN_POINT ( 'NONE',  ( -15.01980243943000026, 9.926543453055000299, 4.231053017515000292 ) ) ;
#22962 = DIRECTION ( 'NONE',  ( 1.000000000000000000, 0.000000000000000000, 0.000000000000000000 ) ) ;
#22963 = CARTESIAN_POINT ( 'NONE',  ( 15.87062451746000136, 7.573146751075999994, 6.130183788350000995 ) ) ;
#22964 = DIRECTION ( 'NONE',  ( 1.000000000000000000, 0.000000000000000000, 0.000000000000000000 ) ) ;
#22965 = DIRECTION ( 'NONE',  ( 0.000000000000000000, 1.000000000000000000, 0.000000000000000000 ) ) ;
#22966 = CARTESIAN_POINT ( 'NONE',  ( 20.84425946885999892, 10.21728774804000039, -0.02082316127604999859 ) ) ;
#22967 = ORIENTED_EDGE ( 'NONE', *, *, #5676, .F. ) ;
#22968 = VECTOR ( 'NONE', #19463, 1000.000000000000000 ) ;
#22969 = CARTESIAN_POINT ( 'NONE',  ( 18.43276763470113977, -1.730528564387503687, 9.411642275345988295 ) ) ;
#22970 = CARTESIAN_POINT ( 'NONE',  ( 2.429928970624000151, 28.22663313894999959, 0.4339301335947000626 ) ) ;
#22971 = CARTESIAN_POINT ( 'NONE',  ( -2.590695557940999816, 11.85722059114999638, 3.971571042362003645 ) ) ;
#22972 = CARTESIAN_POINT ( 'NONE',  ( 2.050437535749142448, 28.96303242407652689, 0.6788312481738240090 ) ) ;
#22973 = EDGE_CURVE ( 'NONE', #18970, #7614, #7059, .T. ) ;
#22974 = CARTESIAN_POINT ( 'NONE',  ( -14.42210300337531770, 4.045542311194462393, -8.116575561360184210 ) ) ;
#22975 = CARTESIAN_POINT ( 'NONE',  ( -19.91018437026999877, -4.577733189479999965, 10.05552272314999840 ) ) ;
#22976 = DIRECTION ( 'NONE',  ( -1.000000000000000000, 0.000000000000000000, 0.000000000000000000 ) ) ;
#22977 = AXIS2_PLACEMENT_3D ( 'NONE', #16364, #5126, #10574 ) ;
#22978 = EDGE_LOOP ( 'NONE', ( #22203, #6666, #7924, #14303 ) ) ;
#22979 = CARTESIAN_POINT ( 'NONE',  ( -4.900699999999999612, 1.284663064832999817E-14, 0.000000000000000000 ) ) ;
#22980 = CARTESIAN_POINT ( 'NONE',  ( -4.749997084077000054, 12.55000000011000161, -4.491085162427999259E-09 ) ) ;
#22981 = CARTESIAN_POINT ( 'NONE',  ( -4.276707022270998415, 13.50735784737998735, 4.819750607759997862 ) ) ;
#22982 = CARTESIAN_POINT ( 'NONE',  ( -1.105760685111225161, 6.867277184477957874, 1.356840241705358663 ) ) ;
#22983 = CARTESIAN_POINT ( 'NONE',  ( 0.000000000000000000, 29.69999999999999929, 0.000000000000000000 ) ) ;
#22984 = ADVANCED_FACE ( 'NONE', ( #13458 ), #14427, .F. ) ;
#22985 = CARTESIAN_POINT ( 'NONE',  ( -6.089787304710518434, 16.07459693448465998, -1.026727111026596528 ) ) ;
#22986 = CARTESIAN_POINT ( 'NONE',  ( 12.92793875730999886, -7.038709952280000515, 5.788476981990000603 ) ) ;
#22987 = CARTESIAN_POINT ( 'NONE',  ( -0.6543697108981931798, 27.36666666666666359, 2.434931691670791043 ) ) ;
#22988 = ORIENTED_EDGE ( 'NONE', *, *, #5402, .F. ) ;
#22989 = DIRECTION ( 'NONE',  ( 0.000000000000000000, 1.000000000000000000, 0.000000000000000000 ) ) ;
#22990 = LINE ( 'NONE', #835, #15314 ) ;
#22991 = CARTESIAN_POINT ( 'NONE',  ( 1.004156133560362374, 13.74043590524155611, -6.042168540479655903 ) ) ;
#22992 = CIRCLE ( 'NONE', #16823, 2.750000000000000000 ) ;
#22993 = ORIENTED_EDGE ( 'NONE', *, *, #17257, .T. ) ;
#22994 = CARTESIAN_POINT ( 'NONE',  ( 4.000000000000000000, 28.30000000000000071, 2.309401076759000304 ) ) ;
#22995 = FILL_AREA_STYLE_COLOUR ( '', #5754 ) ;
#22996 = CARTESIAN_POINT ( 'NONE',  ( 2.675893616224000127, 28.54543090945000117, 0.6150008616569999642 ) ) ;
#22997 = CARTESIAN_POINT ( 'NONE',  ( 14.40587415921926251, -4.504273601744794853, 7.838925639499337628 ) ) ;
#22998 = CARTESIAN_POINT ( 'NONE',  ( 14.44790149212718156, 6.135938681383620974, -8.358155082646094414 ) ) ;
#22999 = CARTESIAN_POINT ( 'NONE',  ( -4.364381710089920929, 13.57203098063190438, 4.996831629903377703 ) ) ;
#23000 = CARTESIAN_POINT ( 'NONE',  ( 2.000000000000000000, 26.50000000000000355, -3.464101615137999968 ) ) ;
#23001 = EDGE_CURVE ( 'NONE', #4139, #12867, #20585, .T. ) ;
#23002 = CARTESIAN_POINT ( 'NONE',  ( -2.434931691670790155, 29.80086340285666680, -0.6543697108981963995 ) ) ;
#23003 = ORIENTED_EDGE ( 'NONE', *, *, #11455, .F. ) ;
#23004 = CARTESIAN_POINT ( 'NONE',  ( 0.000000000000000000, 26.34999999328000087, -2.249999993279999888 ) ) ;
#23005 = EDGE_CURVE ( 'NONE', #6143, #22927, #852, .T. ) ;
#23006 = CARTESIAN_POINT ( 'NONE',  ( 11.78924557933399875, -8.668821331392315699, 9.985146724267631058 ) ) ;
#23007 = ORIENTED_EDGE ( 'NONE', *, *, #5844, .F. ) ;
#23008 = CARTESIAN_POINT ( 'NONE',  ( -9.042815982636001948, 20.50000000000000000, 55.76088950527000065 ) ) ;
#23009 = CARTESIAN_POINT ( 'NONE',  ( -2.156733561231868990, 24.62730423855435902, 0.3971439080199647975 ) ) ;
#23010 = CARTESIAN_POINT ( 'NONE',  ( 2.490045692465482574, 13.01343478852942326, 6.243790476444181614 ) ) ;
#23011 = CIRCLE ( 'NONE', #15642, 3.000000000000000000 ) ;
#23012 = CARTESIAN_POINT ( 'NONE',  ( 6.146720786676755033, 14.15407065691313093, -0.1974862381914592735 ) ) ;
#23013 = CARTESIAN_POINT ( 'NONE',  ( -5.790975589382995281, 15.02417427529998939, -3.017301706163999953 ) ) ;
#23014 = DIRECTION ( 'NONE',  ( 0.000000000000000000, 0.000000000000000000, -1.000000000000000000 ) ) ;
#23015 = EDGE_CURVE ( 'NONE', #7090, #1524, #8874, .T. ) ;
#23016 = ORIENTED_EDGE ( 'NONE', *, *, #19554, .T. ) ;
#23017 = ORIENTED_EDGE ( 'NONE', *, *, #11622, .F. ) ;
#23018 = ADVANCED_FACE ( 'NONE', ( #8986 ), #13626, .F. ) ;
#23019 = CARTESIAN_POINT ( 'NONE',  ( -2.321186682587942141, 30.00000000000000355, -3.278664397485417048 ) ) ;
#23020 = CARTESIAN_POINT ( 'NONE',  ( -0.4976720038370057164, 6.795687889532847414, -1.678983103574156699 ) ) ;
#23021 = DIRECTION ( 'NONE',  ( 0.9947502446910230223, 0.000000000000000000, -0.1023325494999024060 ) ) ;
#23022 = ORIENTED_EDGE ( 'NONE', *, *, #4912, .F. ) ;
#23023 = CARTESIAN_POINT ( 'NONE',  ( 0.000000000000000000, 28.15000000000000213, -4.309401076758999416 ) ) ;
#23024 = CARTESIAN_POINT ( 'NONE',  ( 6.159835994203606724, 14.07226188649447707, 0.4016429018227478109 ) ) ;
#23025 = CARTESIAN_POINT ( 'NONE',  ( 15.16948588246496854, 6.616435942061880127, 7.943911616450581192 ) ) ;
#23026 = CARTESIAN_POINT ( 'NONE',  ( -15.45409440152999991, 1.691041824560000073, -10.90062380652000051 ) ) ;
#23027 = AXIS2_PLACEMENT_3D ( 'NONE', #11689, #23050, #17251 ) ;
#23028 = CARTESIAN_POINT ( 'NONE',  ( 0.000000000000000000, 9.050044887908999414, 0.000000000000000000 ) ) ;
#23029 = CARTESIAN_POINT ( 'NONE',  ( -20.45858076833473049, 9.968623160409832096, -3.311721528445693785 ) ) ;
#23030 = CIRCLE ( 'NONE', #17226, 4.000000000000000000 ) ;
#23031 = DIRECTION ( 'NONE',  ( 0.000000000000000000, 1.000000000000000000, 0.000000000000000000 ) ) ;
#23032 = CARTESIAN_POINT ( 'NONE',  ( -1.465621426440372410, 29.50897963818352920, 1.586551976367980732 ) ) ;
#23033 = EDGE_LOOP ( 'NONE', ( #14142, #6520, #23912, #20759 ) ) ;
#23034 = CARTESIAN_POINT ( 'NONE',  ( -1.737762083858999995, 25.31592804684000342, 1.580334386437000083 ) ) ;
#23035 = CARTESIAN_POINT ( 'NONE',  ( -16.22830427515723883, -2.009085296611893945, 10.21346353486777048 ) ) ;
#23036 = EDGE_LOOP ( 'NONE', ( #23042, #7129, #17729, #6582 ) ) ;
#23037 = DIRECTION ( 'NONE',  ( 1.000000000000000000, 0.000000000000000000, 0.000000000000000000 ) ) ;
#23038 = CARTESIAN_POINT ( 'NONE',  ( 6.118390120404000321, 14.49807793005001777, -0.4535226805296005415 ) ) ;
#23039 = CARTESIAN_POINT ( 'NONE',  ( -4.820914651057999656, 13.20110358116999905, -5.836454220812999694 ) ) ;
#23040 = DIRECTION ( 'NONE',  ( 1.000000000000000000, 0.000000000000000000, 0.000000000000000000 ) ) ;
#23041 = CARTESIAN_POINT ( 'NONE',  ( 16.13531392131000075, 9.604728693984000643, 1.402583754804999971 ) ) ;
#23042 = ORIENTED_EDGE ( 'NONE', *, *, #23913, .F. ) ;
#23043 = AXIS2_PLACEMENT_3D ( 'NONE', #3258, #22011, #10642 ) ;
#23044 = CARTESIAN_POINT ( 'NONE',  ( -2.434931691670790155, 27.16666666666666785, -0.6543697108981958444 ) ) ;
#23045 = DIRECTION ( 'NONE',  ( -1.000000000000000000, 0.000000000000000000, 0.000000000000000000 ) ) ;
#23046 = VERTEX_POINT ( 'NONE', #17952 ) ;
#23047 = CARTESIAN_POINT ( 'NONE',  ( -4.724999999999999645, 14.90000000000000036, 0.000000000000000000 ) ) ;
#23048 = CARTESIAN_POINT ( 'NONE',  ( 21.58708333333332163, -2.414572076269414946, 8.985188864258029540 ) ) ;
#23049 = CARTESIAN_POINT ( 'NONE',  ( -23.22511994411532754, 9.140896836353345378, -1.774683072962275121 ) ) ;
#23050 = DIRECTION ( 'NONE',  ( 1.000000000000000000, 0.000000000000000000, 0.000000000000000000 ) ) ;
#23051 = CARTESIAN_POINT ( 'NONE',  ( 16.89463950886860744, 8.818331488848656363, 5.668027532568643778 ) ) ;
#23052 = DIRECTION ( 'NONE',  ( 0.000000000000000000, 0.000000000000000000, 1.000000000000000000 ) ) ;
#23053 = CARTESIAN_POINT ( 'NONE',  ( -14.49284524109528682, 11.34356441105102320, -5.352320976844095135 ) ) ;
#23054 = FACE_OUTER_BOUND ( 'NONE', #21224, .T. ) ;
#23055 = FACE_OUTER_BOUND ( 'NONE', #6694, .T. ) ;
#23056 = CARTESIAN_POINT ( 'NONE',  ( -4.544340308300998998, 13.49051417780999884, -5.132142894851999593 ) ) ;
#23057 = CYLINDRICAL_SURFACE ( 'NONE', #22299, 1.000000000000000222 ) ;
#23058 = CARTESIAN_POINT ( 'NONE',  ( -1.237648089123723594, 30.08161986502327423, -1.770177328435171393 ) ) ;
#23059 = VERTEX_POINT ( 'NONE', #21710 ) ;
#23060 = CARTESIAN_POINT ( 'NONE',  ( 20.03377367193000325, 4.847508016323000213, 9.108486939822999062 ) ) ;
#23061 = CARTESIAN_POINT ( 'NONE',  ( 23.67568178759826836, 5.018981409586317000, -9.344864196030615133 ) ) ;
#23062 = CARTESIAN_POINT ( 'NONE',  ( -10.34021276376999943, 7.100000000000000533, 0.000000000000000000 ) ) ;
#23063 = DIRECTION ( 'NONE',  ( 0.9970458808888235103, 0.000000000000000000, 0.07680827691486176445 ) ) ;
#23064 = CARTESIAN_POINT ( 'NONE',  ( -23.99212502904755340, -13.39645431917461771, -1.796660477931302680 ) ) ;
#23065 = CARTESIAN_POINT ( 'NONE',  ( -0.6109688586221994067, 11.46768424835998168, -4.905989630836000259 ) ) ;
#23066 = ORIENTED_EDGE ( 'NONE', *, *, #20459, .T. ) ;
#23067 = CARTESIAN_POINT ( 'NONE',  ( -15.78639678782281131, -9.050916927008973545, 5.383602120784745537 ) ) ;
#23068 = CARTESIAN_POINT ( 'NONE',  ( 0.5364167134210068300, 26.26145275469147222, 2.093854992564738282 ) ) ;
#23069 = CIRCLE ( 'NONE', #18439, 0.09999999999999939493 ) ;
#23070 = CARTESIAN_POINT ( 'NONE',  ( 4.749999884653000493, 20.09999988465641252, -5.093549567505999500E-08 ) ) ;
#23071 = B_SPLINE_CURVE_WITH_KNOTS ( 'NONE', 3,
 ( #22186, #5600, #17093, #7526, #490, #7892, #9239, #13331, #20730, #22652, #26, #16726 ),
 .UNSPECIFIED., .F., .F.,
 ( 4, 2, 2, 2, 2, 4 ),
 ( 0.000000000000000000, 0.2499999999999920064, 0.3749999999999807931, 0.4374999999999751865, 0.4999999999999695799, 1.000000000000000000 ),
 .UNSPECIFIED. ) ;
#23072 = AXIS2_PLACEMENT_3D ( 'NONE', #1911, #22239, #20672 ) ;
#23073 = CYLINDRICAL_SURFACE ( 'NONE', #14463, 10.59999999999999964 ) ;
#23074 = ORIENTED_EDGE ( 'NONE', *, *, #9654, .T. ) ;
#23075 = CARTESIAN_POINT ( 'NONE',  ( -2.749999993363999806, 22.20000000663619844, 7.185653392336999782E-09 ) ) ;
#23076 = AXIS2_PLACEMENT_3D ( 'NONE', #19553, #15532, #11920 ) ;
#23077 = CARTESIAN_POINT ( 'NONE',  ( 15.96881424931000026, -5.728615299830999597, -9.061514726575000012 ) ) ;
#23078 = CARTESIAN_POINT ( 'NONE',  ( -23.52518536351999856, -7.578138410264999791, 7.542607835675000594 ) ) ;
#23079 = EDGE_CURVE ( 'NONE', #7890, #15169, #1358, .T. ) ;
#23080 = CARTESIAN_POINT ( 'NONE',  ( -14.27333148495000081, -7.281001511342000576, -7.192128478635999578 ) ) ;
#23081 = CARTESIAN_POINT ( 'NONE',  ( -6.332330438508005699, 16.43030572369001874, 1.007229720589999378 ) ) ;
#23082 = CARTESIAN_POINT ( 'NONE',  ( 14.04249951745999958, 7.822669716756000646, 5.722386861447000150 ) ) ;
#23083 = CARTESIAN_POINT ( 'NONE',  ( -1.978431099119786207, 28.65874823216689293, 0.8981439385142484522 ) ) ;
#23084 = DIRECTION ( 'NONE',  ( -0.000000000000000000, 1.000000000000000000, 0.000000000000000000 ) ) ;
#23085 = FACE_OUTER_BOUND ( 'NONE', #18679, .T. ) ;
#23086 = ORIENTED_EDGE ( 'NONE', *, *, #15428, .F. ) ;
#23087 = DIRECTION ( 'NONE',  ( 0.000000000000000000, 1.000000000000000000, 0.000000000000000000 ) ) ;
#23088 = CARTESIAN_POINT ( 'NONE',  ( -2.583184600869000036, 28.72206776951999885, -0.6741018852137000694 ) ) ;
#23089 = CONICAL_SURFACE ( 'NONE', #20022, 7.249999994591000529, 0.7853981633972997312 ) ;
#23090 = CARTESIAN_POINT ( 'NONE',  ( -2.630645692287001847, 11.80156308281999067, 4.013429856067998180 ) ) ;
#23091 = CARTESIAN_POINT ( 'NONE',  ( -19.39549577250665280, 8.011803281376410624, -4.617569357475225011 ) ) ;
#23092 = CARTESIAN_POINT ( 'NONE',  ( -14.36261680801592000, 5.626503938841797670, -7.110814111431843720 ) ) ;
#23093 = EDGE_CURVE ( 'NONE', #1412, #10853, #3912, .T. ) ;
#23094 = CARTESIAN_POINT ( 'NONE',  ( -22.08228346541999798, 8.068880685816999687, 7.633144572907999859 ) ) ;
#23095 = AXIS2_PLACEMENT_3D ( 'NONE', #4324, #4444, #11715 ) ;
#23096 = CARTESIAN_POINT ( 'NONE',  ( 0.000000000000000000, 0.000000000000000000, 0.000000000000000000 ) ) ;
#23097 = EDGE_LOOP ( 'NONE', ( #1194, #19762, #17929, #12144 ) ) ;
#23098 = DIRECTION ( 'NONE',  ( 0.000000000000000000, -1.000000000000000000, 0.000000000000000000 ) ) ;
#23099 = CARTESIAN_POINT ( 'NONE',  ( 4.647821725315998798, 14.83942339102000041, 4.018338400731999549 ) ) ;
#23100 = CARTESIAN_POINT ( 'NONE',  ( -10.90000000000000036, 10.59999999999999964, 0.000000000000000000 ) ) ;
#23101 = DIRECTION ( 'NONE',  ( -0.7071067811905932254, 0.7071067811824932603, -1.099460837533990473E-07 ) ) ;
#23102 = CARTESIAN_POINT ( 'NONE',  ( -9.988839711695000290, -15.41946301301999966, 2.151533345712000056 ) ) ;
#23103 = DIRECTION ( 'NONE',  ( -1.000000000000000000, 0.000000000000000000, 0.000000000000000000 ) ) ;
#23104 = AXIS2_PLACEMENT_3D ( 'NONE', #2170, #16943, #10048 ) ;
#23105 = AXIS2_PLACEMENT_3D ( 'NONE', #8415, #10598, #17983 ) ;
#23106 = CARTESIAN_POINT ( 'NONE',  ( 12.05043875730999936, 7.573215573255999367, -5.027566056405999184 ) ) ;
#23107 = CARTESIAN_POINT ( 'NONE',  ( 24.48327518124253643, 1.286795374954478932, 12.49999999999999822 ) ) ;
#23108 = ADVANCED_FACE ( 'NONE', ( #8747 ), #6925, .F. ) ;
#23109 = ORIENTED_EDGE ( 'NONE', *, *, #21823, .F. ) ;
#23110 = CARTESIAN_POINT ( 'NONE',  ( 2.500000000000000000, 28.40000000000000213, 0.000000000000000000 ) ) ;
#23111 = CARTESIAN_POINT ( 'NONE',  ( 0.9599026219552000416, 30.10507675623999901, -2.343868003748000195 ) ) ;
#23112 = DIRECTION ( 'NONE',  ( -1.000000000000000000, 0.000000000000000000, 0.000000000000000000 ) ) ;
#23113 = CARTESIAN_POINT ( 'NONE',  ( -2.865402830231887243, 14.08554499887472566, -5.425456058132048121 ) ) ;
#23114 = DIRECTION ( 'NONE',  ( 0.000000000000000000, 0.000000000000000000, -1.000000000000000000 ) ) ;
#23115 = DIRECTION ( 'NONE',  ( 0.000000000000000000, -0.7071067811866525998, -0.7071067811864425456 ) ) ;
#23116 = CARTESIAN_POINT ( 'NONE',  ( 0.1597943784973999970, 29.98160862143000216, 2.741012656831999905 ) ) ;
#23117 = DIRECTION ( 'NONE',  ( 0.000000000000000000, -1.000000000000000000, 0.000000000000000000 ) ) ;
#23118 = CARTESIAN_POINT ( 'NONE',  ( 14.47577869003221451, 6.916416855222763616, -7.723673430031631426 ) ) ;
#23119 = CARTESIAN_POINT ( 'NONE',  ( -4.510025733234193979, 13.50215798145615942, 5.101579666907003485 ) ) ;
#23120 = CARTESIAN_POINT ( 'NONE',  ( -21.13391243917332218, 8.973862284426854075, -2.411528142513474915 ) ) ;
#23121 = EDGE_CURVE ( 'NONE', #20808, #7280, #23381, .T. ) ;
#23122 = CARTESIAN_POINT ( 'NONE',  ( 0.000000000000000000, 21.50000000000000000, 0.000000000000000000 ) ) ;
#23123 = ORIENTED_EDGE ( 'NONE', *, *, #3498, .F. ) ;
#23124 = FACE_OUTER_BOUND ( 'NONE', #6747, .T. ) ;
#23125 = FACE_OUTER_BOUND ( 'NONE', #9526, .T. ) ;
#23126 = CONICAL_SURFACE ( 'NONE', #3800, 1.449999902385000095, 0.7853981633972997312 ) ;
#23127 = ORIENTED_EDGE ( 'NONE', *, *, #17568, .F. ) ;
#23128 = CARTESIAN_POINT ( 'NONE',  ( 1.709519496923999959, 25.75266659807000025, 1.617190848266999881 ) ) ;
#23129 = CARTESIAN_POINT ( 'NONE',  ( -1.042632460611140788, 24.73976796275902146, 1.891962004173780576 ) ) ;
#23130 = CARTESIAN_POINT ( 'NONE',  ( -0.8063831873887827850, 12.82547172164913718, 6.621239620338749354 ) ) ;
#23131 = DIRECTION ( 'NONE',  ( 0.000000000000000000, 1.000000000000000000, 0.000000000000000000 ) ) ;
#23132 = DIRECTION ( 'NONE',  ( -1.000000000000000000, 0.000000000000000000, 0.000000000000000000 ) ) ;
#23133 = ADVANCED_FACE ( 'NONE', ( #23746 ), #12735, .F. ) ;
#23134 = CIRCLE ( 'NONE', #2253, 7.000000000000000000 ) ;
#23135 = CARTESIAN_POINT ( 'NONE',  ( 1.777466727206999941, 26.28919433609999956, -2.254705796085000102 ) ) ;
#23136 = ORIENTED_EDGE ( 'NONE', *, *, #5128, .F. ) ;
#23137 = CIRCLE ( 'NONE', #6519, 2.100000000000000089 ) ;
#23138 = CARTESIAN_POINT ( 'NONE',  ( -14.00000000000000000, -10.27687089286999900, -0.6428416445564000270 ) ) ;
#23139 = CIRCLE ( 'NONE', #18893, 4.750000000000000000 ) ;
#23140 = CARTESIAN_POINT ( 'NONE',  ( -1.540963341621564675, 6.950233192468949106, -0.8594630492748885908 ) ) ;
#23141 = FACE_OUTER_BOUND ( 'NONE', #5953, .T. ) ;
#23142 = EDGE_CURVE ( 'NONE', #11779, #3740, #22892, .T. ) ;
#23143 = ORIENTED_EDGE ( 'NONE', *, *, #6587, .T. ) ;
#23144 = CARTESIAN_POINT ( 'NONE',  ( -20.36066747213000028, -5.792492153153000700, -8.346631074955999097 ) ) ;
#23145 = ADVANCED_FACE ( 'NONE', ( #12392 ), #17499, .T. ) ;
#23146 = DIRECTION ( 'NONE',  ( 0.000000000000000000, 0.4362437346113740011, -0.8998285414523820025 ) ) ;
#23147 = CARTESIAN_POINT ( 'NONE',  ( 20.52891666666666026, -2.407698974803198055, -8.958643823178077170 ) ) ;
#23148 = CARTESIAN_POINT ( 'NONE',  ( 15.21050474296684740, 5.394461060204293723, 8.833667902654472215 ) ) ;
#23149 = CIRCLE ( 'NONE', #4596, 7.500000000000000000 ) ;
#23150 = CARTESIAN_POINT ( 'NONE',  ( -16.17674766165999856, -7.868860569998000543, 7.758953960773999903 ) ) ;
#23151 = CARTESIAN_POINT ( 'NONE',  ( 1.452663470816000002, 28.93738057083000115, -1.855135613986000021 ) ) ;
#23152 = CARTESIAN_POINT ( 'NONE',  ( -22.56483322422616311, -4.636276520427093928, 8.029449324473102223 ) ) ;
#23153 = CARTESIAN_POINT ( 'NONE',  ( -4.720309893115999245, 12.53493801369999616, 0.1499651499519998876 ) ) ;
#23154 = CARTESIAN_POINT ( 'NONE',  ( -14.45834475453999879, 5.064797291421999859, 10.11313827054000036 ) ) ;
#23155 = AXIS2_PLACEMENT_3D ( 'NONE', #9362, #16735, #146 ) ;
#23156 = CARTESIAN_POINT ( 'NONE',  ( -1.716601787089840903, 29.32076057752635734, -1.311645278114084823 ) ) ;
#23157 = EDGE_CURVE ( 'NONE', #8416, #1912, #13235, .T. ) ;
#23158 = ORIENTED_EDGE ( 'NONE', *, *, #5798, .T. ) ;
#23159 = CARTESIAN_POINT ( 'NONE',  ( -6.042815432463000569, 16.37762245475000000, 0.9999999720525000191 ) ) ;
#23160 = CARTESIAN_POINT ( 'NONE',  ( -15.27331153816034970, 3.763286766049342091, -9.840476004715160485 ) ) ;
#23161 = VECTOR ( 'NONE', #15303, 1000.000000000000000 ) ;
#23162 = B_SPLINE_CURVE_WITH_KNOTS ( 'NONE', 3,
 ( #2892, #1190, #1314, #2770, #23338, #13901, #12339, #10156, #3142, #15701 ),
 .UNSPECIFIED., .F., .F.,
 ( 4, 1, 1, 2, 2, 4 ),
 ( 0.000000000000000000, 0.2500000000000000000, 0.3749999999999996114, 0.4374999999999996669, 0.4999999999999996669, 1.000000000000000000 ),
 .UNSPECIFIED. ) ;
#23163 = VERTEX_POINT ( 'NONE', #5464 ) ;
#23164 = CARTESIAN_POINT ( 'NONE',  ( 6.641840470203004720, 13.49927717272000294, -0.1936058750606000356 ) ) ;
#23165 = CARTESIAN_POINT ( 'NONE',  ( 11.99999999999999822, 0.8847351093544478795, -8.935637287590818545 ) ) ;
#23166 = AXIS2_PLACEMENT_3D ( 'NONE', #3254, #22471, #20427 ) ;
#23167 = CARTESIAN_POINT ( 'NONE',  ( 24.07420734439638821, 5.678657336858167426, -12.50000000000000355 ) ) ;
#23168 = CARTESIAN_POINT ( 'NONE',  ( 13.39312642131000075, -9.609817522467999140, -0.6894128909195000876 ) ) ;
#23169 = ORIENTED_EDGE ( 'NONE', *, *, #2737, .F. ) ;
#23170 = CARTESIAN_POINT ( 'NONE',  ( 0.000000000000000000, 30.50000000000000000, 0.000000000000000000 ) ) ;
#23171 = DIRECTION ( 'NONE',  ( 0.000000000000000000, 0.000000000000000000, -1.000000000000000000 ) ) ;
#23172 = SURFACE_STYLE_USAGE ( .BOTH. , #16139 ) ;
#23173 = CIRCLE ( 'NONE', #23952, 0.9999999999999991118 ) ;
#23174 = ADVANCED_FACE ( 'NONE', ( #20475 ), #19440, .T. ) ;
#23175 = EDGE_LOOP ( 'NONE', ( #1507, #21810, #13474, #18915, #15834 ) ) ;
#23176 = CARTESIAN_POINT ( 'NONE',  ( -12.50000000000000000, 6.790122574649000597, -5.897138879738999862 ) ) ;
#23177 = CARTESIAN_POINT ( 'NONE',  ( 11.43887872962561048, 9.287405149887408840, 8.913622445536628192 ) ) ;
#23178 = CARTESIAN_POINT ( 'NONE',  ( 44.70988823752291097, 36.26856778792605240, 6.000000000000000000 ) ) ;
#23179 = CARTESIAN_POINT ( 'NONE',  ( -14.00000000000000000, 8.507292963980999545, 3.029321241734000303 ) ) ;
#23181 = CARTESIAN_POINT ( 'NONE',  ( 16.27717232079294263, 0.01447902640547235782, -10.36628560847415059 ) ) ;
#23180 = AXIS2_PLACEMENT_3D ( 'NONE', #6868, #5071, #14140 ) ;
#23182 = CONICAL_SURFACE ( 'NONE', #4630, 9.152445778720998959, 0.02565634000431304615 ) ;
#23183 = CARTESIAN_POINT ( 'NONE',  ( 12.00000000000000355, -4.925392270767085634, -8.318283231588928572 ) ) ;
#23184 = CARTESIAN_POINT ( 'NONE',  ( -14.48633711635906174, 11.53909476760598807, -5.013715100885117515 ) ) ;
#23185 = CARTESIAN_POINT ( 'NONE',  ( 20.27140652306000135, 7.802973122706000630, 8.032991296161000605 ) ) ;
#23186 = DIRECTION ( 'NONE',  ( 0.000000000000000000, 0.000000000000000000, -1.000000000000000000 ) ) ;
#23187 = CARTESIAN_POINT ( 'NONE',  ( -3.796676405536449028, 14.08940060151082108, -4.856290979845076627 ) ) ;
#23188 = CARTESIAN_POINT ( 'NONE',  ( -2.154922498786136398, 30.19489467509957947, -0.1487298284546440252 ) ) ;
#23189 = ADVANCED_FACE ( 'NONE', ( #22275 ), #20586, .T. ) ;
#23190 = VERTEX_POINT ( 'NONE', #16704 ) ;
#23191 = CARTESIAN_POINT ( 'NONE',  ( 21.43909193728000062, 4.096243081809999964, -10.09291015812000047 ) ) ;
#23192 = CARTESIAN_POINT ( 'NONE',  ( 23.53381486928319077, 0.02178524961730664289, -10.60783701616260721 ) ) ;
#23193 = CARTESIAN_POINT ( 'NONE',  ( 4.549999999999859490, 22.00000000000000000, 0.000000000000000000 ) ) ;
#23194 = CIRCLE ( 'NONE', #3821, 5.625000000000000000 ) ;
#23195 = CARTESIAN_POINT ( 'NONE',  ( -0.5347081996567876194, 24.26085803503821836, -2.188906454050921546 ) ) ;
#23196 = CARTESIAN_POINT ( 'NONE',  ( -23.74465998031000069, -13.93375672974000068, -0.8660254037843999608 ) ) ;
#23197 = CARTESIAN_POINT ( 'NONE',  ( -2.649379677059598759, 24.52555747447238943, -3.089210087443399200 ) ) ;
#23198 = VERTEX_POINT ( 'NONE', #18416 ) ;
#23199 = CARTESIAN_POINT ( 'NONE',  ( -14.13963379130298037, -4.565423490151436781, 9.281307119413254370 ) ) ;
#23200 = CARTESIAN_POINT ( 'NONE',  ( -4.000000000000000888, 29.96241504948189771, -0.8002143650531428065 ) ) ;
#23201 = B_SPLINE_CURVE_WITH_KNOTS ( 'NONE', 3,
 ( #11452, #1651, #7809, #20766 ),
 .UNSPECIFIED., .F., .F.,
 ( 4, 4 ),
 ( 0.000000000000000000, 1.000000000000000000 ),
 .UNSPECIFIED. ) ;
#23202 = CONICAL_SURFACE ( 'NONE', #10846, 4.699999872533999756, 0.7853981633972997312 ) ;
#23203 = CARTESIAN_POINT ( 'NONE',  ( 2.066886497620839869, 27.27369194946930619, -0.7492713746921416673 ) ) ;
#23204 = CARTESIAN_POINT ( 'NONE',  ( -10.90000000000000036, 1.358133300253999998E-14, 0.000000000000000000 ) ) ;
#23205 = ORIENTED_EDGE ( 'NONE', *, *, #18856, .T. ) ;
#23206 = CARTESIAN_POINT ( 'NONE',  ( -19.10300673838166574, 0.5074784849211602111, 9.209648430438782896 ) ) ;
#23207 = CARTESIAN_POINT ( 'NONE',  ( -4.622988392615989817, 15.59405543785941006, -4.019176710598885371 ) ) ;
#23208 = CARTESIAN_POINT ( 'NONE',  ( -23.09541789318999960, -10.91273857643000156, 2.518621640306000220 ) ) ;
#23209 = CARTESIAN_POINT ( 'NONE',  ( -18.74219914028000034, 5.524159514902000190, 8.762982706192000038 ) ) ;
#23210 = CARTESIAN_POINT ( 'NONE',  ( -6.214960006199002684, 16.43302743514002628, 1.007233960737000222 ) ) ;
#23211 = CARTESIAN_POINT ( 'NONE',  ( 18.10499951746000136, -5.256258768401999681, 8.277723090073999757 ) ) ;
#23212 = CARTESIAN_POINT ( 'NONE',  ( 1.959918021306048308, 28.26123095495162474, -0.9363544129381041747 ) ) ;
#23213 = FACE_BOUND ( 'NONE', #10956, .T. ) ;
#23214 = CARTESIAN_POINT ( 'NONE',  ( 5.315020105233999814, 13.91583881926999844, -3.802361444130999857 ) ) ;
#23215 = ORIENTED_EDGE ( 'NONE', *, *, #17869, .F. ) ;
#23216 = CARTESIAN_POINT ( 'NONE',  ( -2.126245409042402112, 13.91230505524877614, 5.744102105465449526 ) ) ;
#23217 = CARTESIAN_POINT ( 'NONE',  ( -1.042632460611140788, 24.73976796275902146, 1.891962004173780576 ) ) ;
#23218 = DIRECTION ( 'NONE',  ( 0.000000000000000000, 1.000000000000000000, 0.000000000000000000 ) ) ;
#23219 = CARTESIAN_POINT ( 'NONE',  ( -14.51410574374127904, 1.264063492210389716, -8.954773398761787462 ) ) ;
#23220 = CARTESIAN_POINT ( 'NONE',  ( -23.25187528588000063, -11.01077565003999936, 1.685400950775999940 ) ) ;
#23221 = CARTESIAN_POINT ( 'NONE',  ( 4.750000000000000000, 22.00000000000000000, 0.000000000000000000 ) ) ;
#23222 = ORIENTED_EDGE ( 'NONE', *, *, #11562, .T. ) ;
#23223 = EDGE_CURVE ( 'NONE', #14333, #3424, #9449, .T. ) ;
#23224 = DIRECTION ( 'NONE',  ( 1.000000000000000000, 0.000000000000000000, 0.000000000000000000 ) ) ;
#23225 = CARTESIAN_POINT ( 'NONE',  ( 1.999318247333280896, 11.65229316158473694, -4.385180337949393881 ) ) ;
#23226 = CARTESIAN_POINT ( 'NONE',  ( 1.963372574454999464, 13.97765948033002026, 5.856068077966999574 ) ) ;
#23227 = CARTESIAN_POINT ( 'NONE',  ( 11.77933705839073752, -1.226278748475006397, -8.915936121416093485 ) ) ;
#23228 = CARTESIAN_POINT ( 'NONE',  ( -14.25243324638999809, 6.216878364870000340, 12.50000000000000000 ) ) ;
#23229 = CARTESIAN_POINT ( 'NONE',  ( -11.31253221169000156, -12.85060658243000020, -8.789246050924999665 ) ) ;
#23230 = CARTESIAN_POINT ( 'NONE',  ( -7.834000000000000519, 1.320585629393000037E-14, 0.000000000000000000 ) ) ;
#23231 = CARTESIAN_POINT ( 'NONE',  ( 18.32906392130999862, 1.076221949391999999, 9.704785274157000430 ) ) ;
#23232 = CARTESIAN_POINT ( 'NONE',  ( 18.92316945876704182, 2.674257117273544093, 10.08631798118172718 ) ) ;
#23233 = ORIENTED_EDGE ( 'NONE', *, *, #7146, .F. ) ;
#23234 = CARTESIAN_POINT ( 'NONE',  ( 0.6543697108981982868, 28.56666666666666288, -2.434931691670790155 ) ) ;
#23235 = CARTESIAN_POINT ( 'NONE',  ( -2.514717642077000104, 30.36979563812999672, 0.3022009937774000066 ) ) ;
#23236 = CARTESIAN_POINT ( 'NONE',  ( 0.7071356748185000374, 23.94065862142999990, -2.622386026786000190 ) ) ;
#23237 = CARTESIAN_POINT ( 'NONE',  ( 2.062592510876792851, 13.89940162384647948, -5.767274509907090341 ) ) ;
#23238 = VECTOR ( 'NONE', #7015, 1000.000000000000000 ) ;
#23239 = EDGE_LOOP ( 'NONE', ( #19863, #6879, #17229, #8291 ) ) ;
#23240 = CARTESIAN_POINT ( 'NONE',  ( 0.000000000000000000, 16.89999999999999858, 0.000000000000000000 ) ) ;
#23241 = CARTESIAN_POINT ( 'NONE',  ( -2.948682383037576571, 22.00131761696259503, 1.025729208553000805E-08 ) ) ;
#23242 = CARTESIAN_POINT ( 'NONE',  ( -2.223554292220999873, 29.69437307903999823, -1.610742350496999986 ) ) ;
#23243 = CARTESIAN_POINT ( 'NONE',  ( -5.372793533988000192, 16.07374366253000275, 2.940837684191000001 ) ) ;
#23244 = B_SPLINE_CURVE_WITH_KNOTS ( 'NONE', 3,
 ( #3166, #12246, #8855, #6543, #16091, #16224 ),
 .UNSPECIFIED., .F., .F.,
 ( 4, 2, 4 ),
 ( 5.225908718322005276E-15, 0.0003975433753701282488, 0.0007950867507350306432 ),
 .UNSPECIFIED. ) ;
#23245 = CARTESIAN_POINT ( 'NONE',  ( 15.89751578318907299, -6.116246800416883289, -8.419007581516531502 ) ) ;
#23246 = DIRECTION ( 'NONE',  ( 0.000000000000000000, 1.000000000000000000, 0.000000000000000000 ) ) ;
#23247 = DIRECTION ( 'NONE',  ( 0.000000000000000000, 1.000000000000000000, 0.000000000000000000 ) ) ;
#23248 = DIRECTION ( 'NONE',  ( -1.000000000000000000, 0.000000000000000000, 0.000000000000000000 ) ) ;
#23249 = ORIENTED_EDGE ( 'NONE', *, *, #537, .F. ) ;
#23250 = CARTESIAN_POINT ( 'NONE',  ( 2.000000000000000000, 18.89999999999999858, 5.041407240605999832E-11 ) ) ;
#23251 = CARTESIAN_POINT ( 'NONE',  ( 11.09594815122425437, -11.32305097984590425, 5.387897831760633416 ) ) ;
#23252 = ORIENTED_EDGE ( 'NONE', *, *, #2903, .T. ) ;
#23253 = EDGE_CURVE ( 'NONE', #6263, #19423, #16034, .T. ) ;
#23254 = CARTESIAN_POINT ( 'NONE',  ( -1.545527083999999940, 23.83766312239999863, -2.022132869220999662 ) ) ;
#23255 = FACE_OUTER_BOUND ( 'NONE', #12241, .T. ) ;
#23256 = CARTESIAN_POINT ( 'NONE',  ( 0.1121017584363108860, 12.80188320469649454, 6.666875631454949769 ) ) ;
#23257 = FACE_BOUND ( 'NONE', #17218, .T. ) ;
#23258 = FACE_OUTER_BOUND ( 'NONE', #4373, .T. ) ;
#23259 = CARTESIAN_POINT ( 'NONE',  ( 0.000000000000000000, 24.65000000674550051, -2.249999993254999886 ) ) ;
#23260 = ORIENTED_EDGE ( 'NONE', *, *, #7066, .T. ) ;
#23261 = CARTESIAN_POINT ( 'NONE',  ( 1.536366799937295413, 30.11753006952333322, 1.999167105995444338 ) ) ;
#23262 = CARTESIAN_POINT ( 'NONE',  ( -11.09999999999999964, 6.613190111079999767, -13.46349570337000046 ) ) ;
#23263 = CARTESIAN_POINT ( 'NONE',  ( 6.696152422707000618, 26.50000000000000000, -6.000000000000000000 ) ) ;
#23264 = VERTEX_POINT ( 'NONE', #4112 ) ;
#23265 = EDGE_CURVE ( 'NONE', #16017, #12276, #9406, .T. ) ;
#23266 = CARTESIAN_POINT ( 'NONE',  ( -19.06225528084999965, -10.03758185236999978, -0.2302352342852000133 ) ) ;
#23267 = CARTESIAN_POINT ( 'NONE',  ( -0.6836813991252411737, 28.12756664670459728, -4.224074002601208910 ) ) ;
#23268 = CARTESIAN_POINT ( 'NONE',  ( 15.18932757003898715, 6.036209813893644416, 8.395765448665670760 ) ) ;
#23269 = PLANE ( 'NONE',  #20689 ) ;
#23270 = CARTESIAN_POINT ( 'NONE',  ( 2.268823611850999455, 29.65675077756000277, -0.6357669325499000212 ) ) ;
#23271 = CARTESIAN_POINT ( 'NONE',  ( -22.64045740894113834, -2.421573919205059156, 9.009506293889163686 ) ) ;
#23272 = CARTESIAN_POINT ( 'NONE',  ( -4.503312502202000189, 12.37293047922001499, -1.619280038292999269 ) ) ;
#23273 = ORIENTED_EDGE ( 'NONE', *, *, #16624, .T. ) ;
#23274 = CYLINDRICAL_SURFACE ( 'NONE', #7531, 3.000000000000000000 ) ;
#23275 = EDGE_CURVE ( 'NONE', #13618, #20340, #16824, .T. ) ;
#23276 = AXIS2_PLACEMENT_3D ( 'NONE', #15979, #21812, #2929 ) ;
#23277 = CARTESIAN_POINT ( 'NONE',  ( -1.029500669195184459, 29.54047064446312731, 1.898863408676955356 ) ) ;
#23278 = ORIENTED_EDGE ( 'NONE', *, *, #4833, .T. ) ;
#23279 = CARTESIAN_POINT ( 'NONE',  ( 0.3272492347489343589, 29.38333333333332575, -2.500000000000000444 ) ) ;
#23280 = CARTESIAN_POINT ( 'NONE',  ( -16.80708775212494288, 10.12209424226509746, -2.478698942612353573 ) ) ;
#23281 = ORIENTED_EDGE ( 'NONE', *, *, #19133, .F. ) ;
#23282 = ADVANCED_FACE ( 'NONE', ( #2295 ), #5898, .T. ) ;
#23283 = CARTESIAN_POINT ( 'NONE',  ( 4.825493926286998914, 14.15457440094998987, -4.012025319334002305 ) ) ;
#23284 = CARTESIAN_POINT ( 'NONE',  ( 11.99999999999999822, -6.567735135913689071, -6.123476794215256369 ) ) ;
#23285 = CARTESIAN_POINT ( 'NONE',  ( 17.72694785191000122, -6.871380090573000032, -8.722589323108000059 ) ) ;
#23286 = CARTESIAN_POINT ( 'NONE',  ( -0.3381971108622000011, 27.76756359723999878, 2.445091418594000032 ) ) ;
#23287 = CARTESIAN_POINT ( 'NONE',  ( 16.16175158531000022, 8.345400111538999965, -5.893156809269999741 ) ) ;
#23288 = VERTEX_POINT ( 'NONE', #13075 ) ;
#23289 = CARTESIAN_POINT ( 'NONE',  ( -8.890913992921001707, 5.961159121560999807, -13.23730574134999927 ) ) ;
#23290 = CARTESIAN_POINT ( 'NONE',  ( 24.50000000000000000, 0.000000000000000000, 0.000000000000000000 ) ) ;
#23291 = ORIENTED_EDGE ( 'NONE', *, *, #19656, .F. ) ;
#23292 = ADVANCED_FACE ( 'NONE', ( #16469 ), #870, .T. ) ;
#23293 = CARTESIAN_POINT ( 'NONE',  ( 8.124934037954998800, 1.125145054518999965E-14, 0.000000000000000000 ) ) ;
#23294 = CARTESIAN_POINT ( 'NONE',  ( -18.13088126894000141, 1.446686056264999920E-14, 0.000000000000000000 ) ) ;
#23295 = AXIS2_PLACEMENT_3D ( 'NONE', #12168, #10354, #1146 ) ;
#23296 = CARTESIAN_POINT ( 'NONE',  ( -14.00000000000000533, 5.593944997764537241, 7.525645797716226326 ) ) ;
#23297 = CARTESIAN_POINT ( 'NONE',  ( 16.51941598158408553, 7.761714885866147995, -6.948838952575716377 ) ) ;
#23298 = CARTESIAN_POINT ( 'NONE',  ( -5.618694691383806727, 14.59993743893240037, 4.601122152415220157 ) ) ;
#23299 = CARTESIAN_POINT ( 'NONE',  ( -14.47158023610679933, 11.86027760101404738, -4.457335568564616324 ) ) ;
#23300 = CARTESIAN_POINT ( 'NONE',  ( 1.306994031390692035, 26.46241504948189416, 3.864208797664315576 ) ) ;
#23301 = DIRECTION ( 'NONE',  ( 0.000000000000000000, 0.000000000000000000, -1.000000000000000000 ) ) ;
#23302 = CARTESIAN_POINT ( 'NONE',  ( -2.113979557940886433, 30.23090653331247069, 0.4557372042204370088 ) ) ;
#23303 = VERTEX_POINT ( 'NONE', #7266 ) ;
#23304 = CARTESIAN_POINT ( 'NONE',  ( 2.283928009913000157, 25.78753186594000013, 0.4887283618359000159 ) ) ;
#23305 = CARTESIAN_POINT ( 'NONE',  ( 19.84052273837000158, 9.448312643429998658, 4.133039138847000693 ) ) ;
#23306 = CARTESIAN_POINT ( 'NONE',  ( 22.93797381236814559, -9.336338345241010472, 4.991623801638819025 ) ) ;
#23307 = DIRECTION ( 'NONE',  ( 0.9999999999999997780, -2.086377177501379609E-08, -3.558922666258043983E-16 ) ) ;
#23308 = EDGE_LOOP ( 'NONE', ( #4727, #14371 ) ) ;
#23309 = ADVANCED_FACE ( 'NONE', ( #11275 ), #17516, .T. ) ;
#23310 = DIRECTION ( 'NONE',  ( -1.000000000000000000, 0.000000000000000000, 0.000000000000000000 ) ) ;
#23311 = LINE ( 'NONE', #6727, #11961 ) ;
#23312 = EDGE_CURVE ( 'NONE', #4978, #15509, #15003, .T. ) ;
#23313 = CIRCLE ( 'NONE', #15560, 1.500000000000000000 ) ;
#23314 = CARTESIAN_POINT ( 'NONE',  ( 4.917038878626002862, 12.44025957970000462, -0.1120513407610999462 ) ) ;
#23315 = EDGE_LOOP ( 'NONE', ( #12635, #5558, #20229, #12526 ) ) ;
#23316 = CARTESIAN_POINT ( 'NONE',  ( -15.95386421119776976, -4.621354449514186058, 9.465521188640689587 ) ) ;
#23317 = CARTESIAN_POINT ( 'NONE',  ( 12.49102043323999922, -6.966913015870999537, -12.06696729233999932 ) ) ;
#23318 = ORIENTED_EDGE ( 'NONE', *, *, #18533, .T. ) ;
#23319 = CARTESIAN_POINT ( 'NONE',  ( 1.746727228398754050, 27.31067536807444185, -1.289094695068520702 ) ) ;
#23320 = CARTESIAN_POINT ( 'NONE',  ( -9.000000000000000000, 19.50000000000000000, -2.000000000000000000 ) ) ;
#23321 = VERTEX_POINT ( 'NONE', #5811 ) ;
#23322 = EDGE_CURVE ( 'NONE', #23589, #19360, #480, .T. ) ;
#23323 = CARTESIAN_POINT ( 'NONE',  ( 1.805925435571642979, 26.69999746901650894, 1.797109528431422465 ) ) ;
#23324 = ADVANCED_FACE ( 'NONE', ( #9332 ), #11335, .F. ) ;
#23325 = CARTESIAN_POINT ( 'NONE',  ( 0.000000000000000000, 22.00000000000000000, -3.099999999999983213 ) ) ;
#23326 = CARTESIAN_POINT ( 'NONE',  ( -23.57717794809000011, 3.577206651746999810, 10.62669505086999955 ) ) ;
#23327 = CARTESIAN_POINT ( 'NONE',  ( -14.61354174348999990, -2.554879995948999838, 10.47217342617999947 ) ) ;
#23328 = CARTESIAN_POINT ( 'NONE',  ( 22.22954166666665543, -5.679568043481586059, -7.390219731457483121 ) ) ;
#23329 = CARTESIAN_POINT ( 'NONE',  ( 17.42744494526000310, 7.698988374779999866, 6.881885182000000434 ) ) ;
#23330 = CARTESIAN_POINT ( 'NONE',  ( -10.35615758860000035, 0.000000000000000000, -7.000000000000000000 ) ) ;
#23331 =( GEOMETRIC_REPRESENTATION_CONTEXT ( 3 ) GLOBAL_UNCERTAINTY_ASSIGNED_CONTEXT ( ( #14465 ) ) GLOBAL_UNIT_ASSIGNED_CONTEXT ( ( #11147, #9329, #16821 ) ) REPRESENTATION_CONTEXT ( 'NONE', 'WORKASPACE' ) );
#23332 = CARTESIAN_POINT ( 'NONE',  ( 2.693005968609320622, 26.46241504948188705, -3.063994432611676810 ) ) ;
#23333 = CARTESIAN_POINT ( 'NONE',  ( 15.12470833333332720, -1.186001144903460203, -9.059411538103518069 ) ) ;
#23334 = ORIENTED_EDGE ( 'NONE', *, *, #16060, .T. ) ;
#23335 = CARTESIAN_POINT ( 'NONE',  ( -1.055729715565287385, 26.42936170367563875, -4.009276318043866638 ) ) ;
#23336 = DIRECTION ( 'NONE',  ( 0.000000000000000000, -1.000000000000000000, 0.000000000000000000 ) ) ;
#23337 = CARTESIAN_POINT ( 'NONE',  ( -1.371352433351999744, 26.37413313894999689, 2.052373795670999979 ) ) ;
#23338 = CARTESIAN_POINT ( 'NONE',  ( 3.145406728938545449, 26.39685207198634487, 2.802800731853388516 ) ) ;
#23339 = CARTESIAN_POINT ( 'NONE',  ( -20.43190095651000249, 10.51156571426000141, -3.447590974849000123 ) ) ;
#23340 = CARTESIAN_POINT ( 'NONE',  ( -3.789523947482483113, 12.08245691660683363, 3.002800408178633251 ) ) ;
#23341 = ORIENTED_EDGE ( 'NONE', *, *, #5543, .F. ) ;
#23342 = APPLICATION_CONTEXT ( 'automotive_design' ) ;
#23343 = FACE_OUTER_BOUND ( 'NONE', #23735, .T. ) ;
#23344 = CARTESIAN_POINT ( 'NONE',  ( 1.306883166391199058, 11.55337411466912378, -4.639543142079135762 ) ) ;
#23345 = FACE_OUTER_BOUND ( 'NONE', #1348, .T. ) ;
#23346 = CARTESIAN_POINT ( 'NONE',  ( -20.71230420454666898, -5.655640480365105027, 7.359084460172671704 ) ) ;
#23347 = AXIS2_PLACEMENT_3D ( 'NONE', #18676, #2321, #14791 ) ;
#23348 = DIRECTION ( 'NONE',  ( 0.000000000000000000, 1.000000000000000000, 0.000000000000000000 ) ) ;
#23349 = LINE ( 'NONE', #408, #7679 ) ;
#23350 = CARTESIAN_POINT ( 'NONE',  ( 17.34187642131000118, -3.686089773936000125, -9.013740861256998471 ) ) ;
#23351 = CARTESIAN_POINT ( 'NONE',  ( -23.68078907432000335, -9.459496811531000304, -9.754788243598999975E-09 ) ) ;
#23352 = VERTEX_POINT ( 'NONE', #11066 ) ;
#23353 = CARTESIAN_POINT ( 'NONE',  ( -22.22922847155658843, -5.637976605639000383, 7.349597483169831413 ) ) ;
#23354 = CARTESIAN_POINT ( 'NONE',  ( -0.4795158958135000149, 29.48253446158999935, -2.681298310498000159 ) ) ;
#23355 = AXIS2_PLACEMENT_3D ( 'NONE', #19531, #17467, #19777 ) ;
#23356 = CARTESIAN_POINT ( 'NONE',  ( -14.86049577250666687, -7.910114609640821470, 4.558959672250926687 ) ) ;
#23357 = CARTESIAN_POINT ( 'NONE',  ( 3.079268300026640315, 14.15153817426477012, -5.294691079465464689 ) ) ;
#23358 = ORIENTED_EDGE ( 'NONE', *, *, #12194, .T. ) ;
#23359 = DIRECTION ( 'NONE',  ( -1.000000000000000000, 0.000000000000000000, -9.309561455062024044E-11 ) ) ;
#23360 = CARTESIAN_POINT ( 'NONE',  ( -23.86847083087676324, -13.66493546063248132, 1.331637500039342115 ) ) ;
#23361 = CARTESIAN_POINT ( 'NONE',  ( 6.086261285717811553, 14.38442930254080210, 0.7146526165609166092 ) ) ;
#23362 = CARTESIAN_POINT ( 'NONE',  ( -2.999999964324536972, 20.10000000000040998, -1.175584031498074967E-07 ) ) ;
#23363 = CARTESIAN_POINT ( 'NONE',  ( 16.48293693919926284, 10.26475150931634417, -1.776896041145952454 ) ) ;
#23364 = DIRECTION ( 'NONE',  ( 1.000000000000000000, 0.000000000000000000, 0.000000000000000000 ) ) ;
#23365 = CARTESIAN_POINT ( 'NONE',  ( -4.085036808003000175, 12.14322947999000135, 2.749988504941001999 ) ) ;
#23366 = CARTESIAN_POINT ( 'NONE',  ( -12.25000000000000000, 6.489681479813073750, -13.21205004727046095 ) ) ;
#23367 = ORIENTED_EDGE ( 'NONE', *, *, #6395, .F. ) ;
#23368 = CARTESIAN_POINT ( 'NONE',  ( -14.67977372642998546, -9.047993639170183400, -0.9263344474169592502 ) ) ;
#23369 = CARTESIAN_POINT ( 'NONE',  ( 0.8117579086199240290, 23.79701621662123401, 2.166923507885120781 ) ) ;
#23370 = B_SPLINE_CURVE_WITH_KNOTS ( 'NONE', 3,
 ( #21168, #17536, #4580, #3137, #23214, #11971 ),
 .UNSPECIFIED., .F., .F.,
 ( 4, 1, 1, 4 ),
 ( 0.000000000000000000, 0.3333333333333000081, 0.6666666666667000474, 1.000000000000000000 ),
 .UNSPECIFIED. ) ;
#23371 = ORIENTED_EDGE ( 'NONE', *, *, #19797, .T. ) ;
#23372 = CARTESIAN_POINT ( 'NONE',  ( -1.464281862760000053, 25.33464492091999887, -1.842154207471000005 ) ) ;
#23373 = PLANE ( 'NONE',  #16655 ) ;
#23374 = DIRECTION ( 'NONE',  ( 0.000000000000000000, -1.000000000000000000, 0.000000000000000000 ) ) ;
#23375 = DIRECTION ( 'NONE',  ( 0.000000000000000000, 1.000000000000000000, 0.000000000000000000 ) ) ;
#23376 = CARTESIAN_POINT ( 'NONE',  ( 1.259047450927246903, 27.73333333333333073, -2.184465970885645536 ) ) ;
#23377 = DIRECTION ( 'NONE',  ( -1.000000000000000000, 0.000000000000000000, 0.000000000000000000 ) ) ;
#23378 = ORIENTED_EDGE ( 'NONE', *, *, #6414, .F. ) ;
#23379 = CARTESIAN_POINT ( 'NONE',  ( -1.999167105995446780, 29.91753006952333394, 1.536366799937292305 ) ) ;
#23380 = AXIS2_PLACEMENT_3D ( 'NONE', #8972, #23500, #3413 ) ;
#23381 = LINE ( 'NONE', #1602, #9367 ) ;
#23382 = FACE_OUTER_BOUND ( 'NONE', #21643, .T. ) ;
#23383 = EDGE_LOOP ( 'NONE', ( #9592, #23169, #22547, #19846 ) ) ;
#23384 = CARTESIAN_POINT ( 'NONE',  ( -23.59031210023999847, 7.092207792705000458, 8.788782243285998774 ) ) ;
#23385 = CARTESIAN_POINT ( 'NONE',  ( 20.18879166666666336, -9.189365897221289714, -1.202758235422014543 ) ) ;
#23386 = CARTESIAN_POINT ( 'NONE',  ( 15.08199357210373392, 8.700070515883242095, 5.582766916463140383 ) ) ;
#23387 = CONICAL_SURFACE ( 'NONE', #12944, 4.699999872533999756, 0.7853981633972997312 ) ;
#23388 = CARTESIAN_POINT ( 'NONE',  ( -16.81976253787999909, -9.102909969768001375, 0.000000000000000000 ) ) ;
#23389 = ADVANCED_FACE ( 'NONE', ( #15816 ), #18301, .T. ) ;
#23390 = CARTESIAN_POINT ( 'NONE',  ( 1.737805054697000084, 30.47971342496999725, -1.597568792902000157 ) ) ;
#23391 = CARTESIAN_POINT ( 'NONE',  ( -18.73259798496000172, -8.620928137991000995, 3.072238420002000314 ) ) ;
#23392 = CARTESIAN_POINT ( 'NONE',  ( 4.720309713848997113, 12.53493730558998998, 0.1499515764287999986 ) ) ;
#23393 = ORIENTED_EDGE ( 'NONE', *, *, #4462, .F. ) ;
#23394 = CARTESIAN_POINT ( 'NONE',  ( -14.66147510250999808, 10.41001213865000175, 4.437054729469999792 ) ) ;
#23395 = CARTESIAN_POINT ( 'NONE',  ( -1.317653730136605361, 29.28743615884798501, -1.711479633934526845 ) ) ;
#23396 = EDGE_LOOP ( 'NONE', ( #4901, #5536, #15105, #205 ) ) ;
#23397 = CARTESIAN_POINT ( 'NONE',  ( -0.3272492347489393549, 29.41666666666667140, -2.499999999999999556 ) ) ;
#23398 = AXIS2_PLACEMENT_3D ( 'NONE', #20011, #3432, #10817 ) ;
#23399 = CARTESIAN_POINT ( 'NONE',  ( -16.89390527367012851, 8.934894438370687197, -5.364026527456945637 ) ) ;
#23400 = VERTEX_POINT ( 'NONE', #23325 ) ;
#23401 = CARTESIAN_POINT ( 'NONE',  ( 18.33699999999999974, -9.141845273363999880, 1.095420050962999850E-14 ) ) ;
#23402 = CARTESIAN_POINT ( 'NONE',  ( 11.31235608933160819, -9.572705071928648835, -8.419524251220471101 ) ) ;
#23403 = ADVANCED_FACE ( 'NONE', ( #10514 ), #2638, .F. ) ;
#23404 = CARTESIAN_POINT ( 'NONE',  ( 12.00000000000000000, 3.198220168757963666, -8.391080537878064405 ) ) ;
#23405 = CARTESIAN_POINT ( 'NONE',  ( 13.61040650243000094, -10.56087978152000062, 3.045457193391999606 ) ) ;
#23406 = CARTESIAN_POINT ( 'NONE',  ( 14.07768908531000207, 0.2086024747513000044, -10.15948369482999958 ) ) ;
#23407 = ORIENTED_EDGE ( 'NONE', *, *, #9835, .F. ) ;
#23408 = CARTESIAN_POINT ( 'NONE',  ( -10.01096149291999815, 13.11075716299000149, 6.234477108572999526 ) ) ;
#23409 = PLANE ( 'NONE',  #11706 ) ;
#23410 = CARTESIAN_POINT ( 'NONE',  ( 0.000000000000000000, 0.000000000000000000, 7.500000000000000000 ) ) ;
#23411 = ORIENTED_EDGE ( 'NONE', *, *, #14821, .T. ) ;
#23412 = CARTESIAN_POINT ( 'NONE',  ( -23.37274701946999755, 6.125680067344999813, -7.545173917617000292 ) ) ;
#23413 = DIRECTION ( 'NONE',  ( -1.000000000000000000, 0.000000000000000000, 0.000000000000000000 ) ) ;
#23414 = CARTESIAN_POINT ( 'NONE',  ( 22.52932875793747769, -3.641196223536565135, 9.931222262582332760 ) ) ;
#23415 = AXIS2_PLACEMENT_3D ( 'NONE', #13929, #17198, #22760 ) ;
#23416 = CARTESIAN_POINT ( 'NONE',  ( -6.182361223440762110, 15.05471004068462193, -3.405165877464595869 ) ) ;
#23417 = CARTESIAN_POINT ( 'NONE',  ( 17.14672531740638917, 1.317997890521231952, 10.34275493089012876 ) ) ;
#23418 = CARTESIAN_POINT ( 'NONE',  ( -18.97978743917332878, 5.628138328197398010, 7.323710967538636929 ) ) ;
#23419 = EDGE_CURVE ( 'NONE', #11805, #12236, #14034, .T. ) ;
#23420 = FACE_BOUND ( 'NONE', #11893, .T. ) ;
#23421 = CARTESIAN_POINT ( 'NONE',  ( -4.062644810066652568, 13.79322630918717962, -4.866505382640951005 ) ) ;
#23422 = CARTESIAN_POINT ( 'NONE',  ( -1.500156801936728845, 30.10144942661541023, -1.558200670483578687 ) ) ;
#23423 = ORIENTED_EDGE ( 'NONE', *, *, #511, .F. ) ;
#23424 = CARTESIAN_POINT ( 'NONE',  ( 23.75882644412315869, -9.280857264428881592, 0.6076903218426756847 ) ) ;
#23425 = CARTESIAN_POINT ( 'NONE',  ( 11.66614181937085704, 8.864734480583086551, -9.645689288095473657 ) ) ;
#23426 = DIRECTION ( 'NONE',  ( -1.000000000000000000, 0.000000000000000000, 0.000000000000000000 ) ) ;
#23427 = CARTESIAN_POINT ( 'NONE',  ( -0.3272492347489284192, 27.61753006952333322, 2.500000000000001332 ) ) ;
#23428 = B_SPLINE_CURVE_WITH_KNOTS ( 'NONE', 3,
 ( #3726, #11244, #3613, #2029, #4085, #9181 ),
 .UNSPECIFIED., .F., .F.,
 ( 4, 1, 1, 4 ),
 ( 0.000000000000000000, 0.3333333333333000081, 0.6666666666667000474, 1.000000000000000000 ),
 .UNSPECIFIED. ) ;
#23429 = ORIENTED_EDGE ( 'NONE', *, *, #5373, .F. ) ;
#23430 = DIRECTION ( 'NONE',  ( 1.000000000000000000, 0.000000000000000000, 0.000000000000000000 ) ) ;
#23431 = CIRCLE ( 'NONE', #10678, 3.100000000000000089 ) ;
#23432 = CARTESIAN_POINT ( 'NONE',  ( 23.77835672501372599, -9.281039036324623126, -1.918975276430111748E-05 ) ) ;
#23433 = EDGE_CURVE ( 'NONE', #6008, #6590, #16345, .T. ) ;
#23434 = VECTOR ( 'NONE', #9735, 1000.000000000000000 ) ;
#23435 = CARTESIAN_POINT ( 'NONE',  ( -2.329590180155310719, 24.49999999999985079, -3.273812635903178059 ) ) ;
#23436 = EDGE_LOOP ( 'NONE', ( #7363, #19804, #17156, #16687, #8260, #17955, #2815 ) ) ;
#23437 = CARTESIAN_POINT ( 'NONE',  ( -14.50247987528135774, 7.489765101905747180, 7.283635598514888621 ) ) ;
#23438 = DIRECTION ( 'NONE',  ( 0.9996708941621507138, 0.02565352539215873945, 0.000000000000000000 ) ) ;
#23439 = ORIENTED_EDGE ( 'NONE', *, *, #1705, .T. ) ;
#23440 = CARTESIAN_POINT ( 'NONE',  ( -1.399330729071998958, 26.71894067039222875, -1.658981764594649411 ) ) ;
#23441 = APPLICATION_PROTOCOL_DEFINITION ( 'draft international standard', 'automotive_design', 1998, #8034 ) ;
#23442 = EDGE_CURVE ( 'NONE', #16718, #12435, #22386, .T. ) ;
#23443 = CARTESIAN_POINT ( 'NONE',  ( -14.37382046148723802, -4.385283933000476253, -12.49975322911771514 ) ) ;
#23444 = VERTEX_POINT ( 'NONE', #13228 ) ;
#23445 = CARTESIAN_POINT ( 'NONE',  ( -19.50708901484166446, 9.171872063609672665, 1.069867623823596459 ) ) ;
#23446 = CARTESIAN_POINT ( 'NONE',  ( -4.536289218716924587, 15.51665606200187497, -4.115569062310257209 ) ) ;
#23447 = CARTESIAN_POINT ( 'NONE',  ( -22.88283862364999877, -1.372540388790000065, -10.58604782883999995 ) ) ;
#23448 = EDGE_CURVE ( 'NONE', #7987, #22092, #1031, .T. ) ;
#23449 = CARTESIAN_POINT ( 'NONE',  ( -18.94532948824999963, 9.886987204373001603, 3.109815198001999903 ) ) ;
#23450 = CARTESIAN_POINT ( 'NONE',  ( -6.323124832514003479, 16.13723008609998999, 0.9717865035293998810 ) ) ;
#23451 = ADVANCED_FACE ( 'NONE', ( #11664 ), #19458, .F. ) ;
#23452 = CARTESIAN_POINT ( 'NONE',  ( 18.51124951746000136, -9.033937733188000863, -3.841755647517000050 ) ) ;
#23453 = CARTESIAN_POINT ( 'NONE',  ( 0.6971734275731837904, 26.76391587493858637, -2.091919652565851440 ) ) ;
#23454 = VECTOR ( 'NONE', #21083, 1000.000000000000000 ) ;
#23455 = AXIS2_PLACEMENT_3D ( 'NONE', #16025, #21500, #14106 ) ;
#23456 = CARTESIAN_POINT ( 'NONE',  ( 3.643546194520564274, 26.29977277844447414, -2.515199777306226903 ) ) ;
#23457 = CARTESIAN_POINT ( 'NONE',  ( 0.000000000000000000, 20.10000000000000142, 0.000000000000000000 ) ) ;
#23458 = ORIENTED_EDGE ( 'NONE', *, *, #12245, .F. ) ;
#23459 = CARTESIAN_POINT ( 'NONE',  ( -17.19767920454667021, -2.385323164064429680, 8.875382679229677052 ) ) ;
#23460 = CARTESIAN_POINT ( 'NONE',  ( 0.3879374145667575102, 13.69591497976315608, 6.116692095101760707 ) ) ;
#23461 = B_SPLINE_CURVE_WITH_KNOTS ( 'NONE', 3,
 ( #8764, #13962, #8530, #14208, #14084, #5022, #1131, #15888, #23279, #23397, #10583, #21478, #20020, #8890, #18090, #16004, #10701, #23528 ),
 .UNSPECIFIED., .F., .F.,
 ( 4, 2, 2, 2, 2, 2, 2, 2, 4 ),
 ( 0.000000000000000000, 0.1250000000000000555, 0.2500000000000001110, 0.3750000000000000555, 0.5000000000000000000, 0.6249999999999998890, 0.7499999999999998890, 0.8749999999999998890, 1.000000000000000000 ),
 .UNSPECIFIED. ) ;
#23462 = CARTESIAN_POINT ( 'NONE',  ( 1.603022320644999832, 27.24369850838000318, 1.603022320644999832 ) ) ;
#23463 = CARTESIAN_POINT ( 'NONE',  ( 3.099999776787000005, 21.99999977679100027, 5.570936506502000395E-07 ) ) ;
#23464 = CARTESIAN_POINT ( 'NONE',  ( -20.57852255339999914, 10.51534603707000137, -3.448831178700999978 ) ) ;
#23465 = EDGE_CURVE ( 'NONE', #13026, #10425, #7682, .T. ) ;
#23466 = CIRCLE ( 'NONE', #11091, 4.750000000000000000 ) ;
#23467 = EDGE_CURVE ( 'NONE', #21630, #14333, #23845, .T. ) ;
#23468 = CARTESIAN_POINT ( 'NONE',  ( -1.983357808483588114, 11.65004507716673210, 4.390781508571285130 ) ) ;
#23469 = ORIENTED_EDGE ( 'NONE', *, *, #23900, .T. ) ;
#23470 = CONICAL_SURFACE ( 'NONE', #15724, 13.23032192316000000, 1.235249617460683957 ) ;
#23471 = LINE ( 'NONE', #6880, #12253 ) ;
#23472 = CARTESIAN_POINT ( 'NONE',  ( 3.895813302869969519, 12.11565003950416397, -2.865938779683453230 ) ) ;
#23473 = CARTESIAN_POINT ( 'NONE',  ( 24.03164415829611400, -5.349159599255311370, -7.707290229052887298 ) ) ;
#23474 = CARTESIAN_POINT ( 'NONE',  ( 23.99062354302999722, -13.93375672974000068, -0.8660254037843999608 ) ) ;
#23475 = EDGE_LOOP ( 'NONE', ( #23732, #20658, #11207, #8001 ) ) ;
#23476 = CARTESIAN_POINT ( 'NONE',  ( -2.499999999999988898, 24.01666666666666217, 0.3272492347490136844 ) ) ;
#23477 = CARTESIAN_POINT ( 'NONE',  ( -6.052215895878795493, 16.24384873199515411, -0.9999999999999972244 ) ) ;
#23478 = B_SPLINE_CURVE_WITH_KNOTS ( 'NONE', 3,
 ( #15251, #20495, #13323, #1961, #7883, #13443, #7766, #18904, #20374, #9346 ),
 .UNSPECIFIED., .F., .F.,
 ( 4, 1, 1, 2, 2, 4 ),
 ( 0.000000000000000000, 0.2500000000000011102, 0.3750000000000014433, 0.4375000000000015543, 0.5000000000000016653, 1.000000000000000000 ),
 .UNSPECIFIED. ) ;
#23479 = CARTESIAN_POINT ( 'NONE',  ( 13.72218892130999990, -3.391610850449999770, -9.027048835217000189 ) ) ;
#23480 = CARTESIAN_POINT ( 'NONE',  ( 18.45312019494581790, 9.917877877953065635, -3.199893147332716126 ) ) ;
#23481 = EDGE_LOOP ( 'NONE', ( #23638, #7797, #3501, #22536, #13687, #12456, #8835, #22541, #11319, #10579 ) ) ;
#23482 = CARTESIAN_POINT ( 'NONE',  ( -22.72066361546963620, 8.032224500089185426, 4.638484310570157199 ) ) ;
#23483 = CARTESIAN_POINT ( 'NONE',  ( -0.7613436424516999423, 28.91384178769000357, 2.298498088615000157 ) ) ;
#23484 = CARTESIAN_POINT ( 'NONE',  ( 0.000000000000000000, 14.90000000000000036, 0.000000000000000000 ) ) ;
#23485 = CARTESIAN_POINT ( 'NONE',  ( 13.49999999999999822, -6.476318932888407431, 7.855616484088395524 ) ) ;
#23486 = AXIS2_PLACEMENT_3D ( 'NONE', #733, #19644, #8139 ) ;
#23487 = ORIENTED_EDGE ( 'NONE', *, *, #23900, .F. ) ;
#23488 = DIRECTION ( 'NONE',  ( 0.000000000000000000, 0.000000000000000000, 1.000000000000000000 ) ) ;
#23489 = CARTESIAN_POINT ( 'NONE',  ( -24.16119556693467985, -12.87912905764661531, 2.692171137954526117 ) ) ;
#23490 = CARTESIAN_POINT ( 'NONE',  ( 5.975075284666832687, 14.41257202741255128, 1.359510027979535574 ) ) ;
#23491 = CARTESIAN_POINT ( 'NONE',  ( -23.69684149972337295, -9.477051524790651271, 0.8648883612165714219 ) ) ;
#23492 = CONICAL_SURFACE ( 'NONE', #10364, 12.68487026514999982, 0.6105562205522639951 ) ;
#23493 = CARTESIAN_POINT ( 'NONE',  ( 14.36426989841201518, 3.489952449228996390, -9.755240512065860514 ) ) ;
#23494 = DIRECTION ( 'NONE',  ( 0.000000000000000000, -1.000000000000000000, 0.000000000000000000 ) ) ;
#23495 = CARTESIAN_POINT ( 'NONE',  ( -3.293058160344002339, 11.97730948580998067, 3.707778763315998649 ) ) ;
#23496 = AXIS2_PLACEMENT_3D ( 'NONE', #7833, #15204, #2497 ) ;
#23497 = PLANE ( 'NONE',  #1910 ) ;
#23498 = EDGE_LOOP ( 'NONE', ( #13352, #9830, #9743, #15959 ) ) ;
#23499 = ADVANCED_FACE ( 'NONE', ( #17342 ), #12027, .T. ) ;
#23500 = DIRECTION ( 'NONE',  ( 0.000000000000000000, -1.000000000000000000, 0.000000000000000000 ) ) ;
#23501 = EDGE_CURVE ( 'NONE', #11154, #9971, #11721, .T. ) ;
#23502 = CARTESIAN_POINT ( 'NONE',  ( -4.000000000000000000, 26.39685207198629158, 1.322601766568779924 ) ) ;
#23503 = ORIENTED_EDGE ( 'NONE', *, *, #18408, .F. ) ;
#23504 = CARTESIAN_POINT ( 'NONE',  ( -2.048929151683000160, 24.67370647670999873, -1.509915493683999799 ) ) ;
#23505 = CARTESIAN_POINT ( 'NONE',  ( 5.905044978160000291, 14.55306956897999981, 1.663656914930999209 ) ) ;
#23506 = DIRECTION ( 'NONE',  ( 0.000000000000000000, 1.000000000000000000, 0.000000000000000000 ) ) ;
#23507 = VECTOR ( 'NONE', #13269, 1000.000000000000000 ) ;
#23508 = CONICAL_SURFACE ( 'NONE', #9582, 9.136555860486998526, 0.02565634000431304615 ) ;
#23509 = CARTESIAN_POINT ( 'NONE',  ( 19.70783333333331910, -0.3412242520863046913, 9.268130979224045163 ) ) ;
#23510 = CARTESIAN_POINT ( 'NONE',  ( 0.3272492347489343589, 27.78333333333333854, -2.500000000000000444 ) ) ;
#23511 = ORIENTED_EDGE ( 'NONE', *, *, #7750, .T. ) ;
#23512 = ADVANCED_BREP_SHAPE_REPRESENTATION ( '', ( #16570, #4390 ), #11350 ) ;
#23513 = CARTESIAN_POINT ( 'NONE',  ( -3.064125534931650296, 29.91068681084918168, -2.849728451093327397 ) ) ;
#23514 = CARTESIAN_POINT ( 'NONE',  ( -0.5252141218270467427, 26.22790185010774522, 2.065890903574498338 ) ) ;
#23515 = DIRECTION ( 'NONE',  ( 0.000000000000000000, 0.000000000000000000, 1.000000000000000000 ) ) ;
#23516 = ORIENTED_EDGE ( 'NONE', *, *, #5980, .T. ) ;
#23517 = CARTESIAN_POINT ( 'NONE',  ( -24.48886857509999970, -10.34867540887999837, -0.7644260386628000115 ) ) ;
#23518 = CARTESIAN_POINT ( 'NONE',  ( -1.835060406388425713, 27.99999999999984723, -3.559329533909752818 ) ) ;
#23519 = CARTESIAN_POINT ( 'NONE',  ( 14.89266383929930093, 10.29194843803560744, -0.9031650063429182973 ) ) ;
#23520 = FACE_OUTER_BOUND ( 'NONE', #7046, .T. ) ;
#23521 = CARTESIAN_POINT ( 'NONE',  ( 2.188113818431999924, 30.33609565378000283, 0.8856361526165000830 ) ) ;
#23522 = CARTESIAN_POINT ( 'NONE',  ( -22.79170577837355438, 2.421737280725368091, 9.013834718038792104 ) ) ;
#23523 = CARTESIAN_POINT ( 'NONE',  ( 3.721017143809998373, 12.17176577897999579, -2.946712179682002386 ) ) ;
#23524 = ORIENTED_EDGE ( 'NONE', *, *, #15881, .F. ) ;
#23525 = VECTOR ( 'NONE', #12634, 1000.000000000000000 ) ;
#23526 = FACE_OUTER_BOUND ( 'NONE', #14244, .T. ) ;
#23527 = VERTEX_POINT ( 'NONE', #17595 ) ;
#23528 = CARTESIAN_POINT ( 'NONE',  ( -2.500000000000000000, 29.60000000000000142, 0.000000000000000000 ) ) ;
#23529 = DIRECTION ( 'NONE',  ( 0.000000000000000000, -1.000000000000000000, 0.000000000000000000 ) ) ;
#23530 = VERTEX_POINT ( 'NONE', #12146 ) ;
#23531 = AXIS2_PLACEMENT_3D ( 'NONE', #16769, #178, #7569 ) ;
#23532 = DIRECTION ( 'NONE',  ( 0.000000000000000000, 1.000000000000000000, 0.000000000000000000 ) ) ;
#23533 = CARTESIAN_POINT ( 'NONE',  ( 16.56079166666665969, -9.096264266808555377, -1.190571260499436512 ) ) ;
#23534 = PLANE ( 'NONE',  #22761 ) ;
#23535 = CIRCLE ( 'NONE', #7290, 3.100000000000000089 ) ;
#23536 = CARTESIAN_POINT ( 'NONE',  ( 18.78333224065999829, -3.764053801582000425, 9.968462294195999718 ) ) ;
#23537 = EDGE_CURVE ( 'NONE', #15489, #13137, #8231, .T. ) ;
#23538 = ORIENTED_EDGE ( 'NONE', *, *, #6317, .T. ) ;
#23539 = CARTESIAN_POINT ( 'NONE',  ( -9.705493992920999347, -2.207063777844999741, 14.34885109169999851 ) ) ;
#23540 = CIRCLE ( 'NONE', #22367, 10.59999999999999964 ) ;
#23541 = CARTESIAN_POINT ( 'NONE',  ( 13.50000000000000000, 7.742518136641512783, 6.218115689482817565 ) ) ;
#23542 = DIRECTION ( 'NONE',  ( -0.5000000000000167644, 0.8660254037844290487, 0.000000000000000000 ) ) ;
#23543 = ORIENTED_EDGE ( 'NONE', *, *, #11048, .T. ) ;
#23544 =( NAMED_UNIT ( * ) PLANE_ANGLE_UNIT ( ) SI_UNIT ( $, .RADIAN. ) );
#23545 = CARTESIAN_POINT ( 'NONE',  ( 11.07373617191558957, 11.07537056389167063, 5.816824279998757063 ) ) ;
#23546 = CARTESIAN_POINT ( 'NONE',  ( 21.02918485986734254, -10.44527410498406006, 1.391412801358522522 ) ) ;
#23547 = CARTESIAN_POINT ( 'NONE',  ( -14.00000000000000355, 7.297470702052054392, 5.625831777954100943 ) ) ;
#23548 = CARTESIAN_POINT ( 'NONE',  ( 17.38903384696896026, -6.833465684892690462, 7.891901893606365626 ) ) ;
#23549 = CARTESIAN_POINT ( 'NONE',  ( -19.09316243917332656, 8.004926875064779068, 4.613896613807892066 ) ) ;
#23550 = CONICAL_SURFACE ( 'NONE', #5749, 13.23032192316000000, 1.235249617460683957 ) ;
#23551 = CARTESIAN_POINT ( 'NONE',  ( 1.409996887616000283, 30.49659672073000038, 1.871210455765000003 ) ) ;
#23552 = CIRCLE ( 'NONE', #14270, 3.000000000000000000 ) ;
#23553 = STYLED_ITEM ( 'NONE', ( #22516 ), #16648 ) ;
#23554 = CARTESIAN_POINT ( 'NONE',  ( -3.999702431747993003, 28.00639765414744531, -0.3779811684369214220 ) ) ;
#23555 = CARTESIAN_POINT ( 'NONE',  ( 1.600079875324325940, 29.89762239541055422, -1.452365398962871312 ) ) ;
#23556 = CLOSED_SHELL ( 'NONE', ( #11471, #8370, #21071, #16886, #20295, #11833, #13905 ) ) ;
#23557 = ORIENTED_EDGE ( 'NONE', *, *, #13827, .T. ) ;
#23558 = CARTESIAN_POINT ( 'NONE',  ( 11.97297107869919586, 13.24884602490437935, -2.052424400535973970 ) ) ;
#23559 = CARTESIAN_POINT ( 'NONE',  ( 23.87429547323717927, 9.821396689478271824, -4.029826075455165579 ) ) ;
#23560 = DIRECTION ( 'NONE',  ( -1.000000000000000000, 0.000000000000000000, 0.000000000000000000 ) ) ;
#23561 = TOROIDAL_SURFACE ( 'NONE', #17362, 2.500000000000000000, 0.5500000000000000444 ) ;
#23562 = ORIENTED_EDGE ( 'NONE', *, *, #13837, .F. ) ;
#23563 = DIRECTION ( 'NONE',  ( 0.000000000000000000, -1.000000000000000000, 0.000000000000000000 ) ) ;
#23564 = CARTESIAN_POINT ( 'NONE',  ( 4.877087740424957296, 14.45533858427638840, -3.799144659019715764 ) ) ;
#23565 = CARTESIAN_POINT ( 'NONE',  ( -3.633619105303003138, 12.00370723790998539, -3.205740308949000639 ) ) ;
#23566 = ORIENTED_EDGE ( 'NONE', *, *, #1275, .T. ) ;
#23567 = VECTOR ( 'NONE', #19389, 1000.000000000000114 ) ;
#23568 = EDGE_CURVE ( 'NONE', #15097, #15539, #15632, .T. ) ;
#23569 = CARTESIAN_POINT ( 'NONE',  ( 12.50898080071999985, -7.466894666658999924, -11.77830275166999918 ) ) ;
#23570 = VERTEX_POINT ( 'NONE', #864 ) ;
#23571 = VECTOR ( 'NONE', #6664, 1000.000000000000000 ) ;
#23572 = CARTESIAN_POINT ( 'NONE',  ( -0.4677043798615876380, 26.65730163938367525, -2.152092775777489475 ) ) ;
#23573 = CIRCLE ( 'NONE', #4241, 6.125000000000002665 ) ;
#23574 = APPLICATION_PROTOCOL_DEFINITION ( 'draft international standard', 'automotive_design', 1998, #23342 ) ;
#23575 = DIRECTION ( 'NONE',  ( -1.000000000000000000, 0.000000000000000000, 0.000000000000000000 ) ) ;
#23576 = ORIENTED_EDGE ( 'NONE', *, *, #13514, .T. ) ;
#23577 = CARTESIAN_POINT ( 'NONE',  ( 1.410165095533915336, 26.67499683627062979, 2.121886834720800419 ) ) ;
#23578 = CIRCLE ( 'NONE', #2695, 9.287173237303996132 ) ;
#23579 = CARTESIAN_POINT ( 'NONE',  ( -4.252372020903545824, 15.23278328154970218, -4.409552293429433334 ) ) ;
#23580 = CARTESIAN_POINT ( 'NONE',  ( -20.79521171905999921, 7.755012229217999931, -7.253067937808999943 ) ) ;
#23581 = EDGE_CURVE ( 'NONE', #15097, #15489, #6523, .T. ) ;
#23582 = CARTESIAN_POINT ( 'NONE',  ( -18.40198888174000302, -9.811392118899000536, 0.2208054555764999982 ) ) ;
#23583 = CARTESIAN_POINT ( 'NONE',  ( -7.500000000000000000, 24.99999999999999645, -6.000000000000000000 ) ) ;
#23584 = CARTESIAN_POINT ( 'NONE',  ( -24.47326038496474965, -0.9464271205007054322, -10.56558464230831618 ) ) ;
#23585 = CARTESIAN_POINT ( 'NONE',  ( 2.147641545635635030, 26.57840781165250021, 0.4457964343191409551 ) ) ;
#23586 = CARTESIAN_POINT ( 'NONE',  ( 0.000000000000000000, 30.00000000000000000, 0.000000000000000000 ) ) ;
#23587 = AXIS2_PLACEMENT_3D ( 'NONE', #18142, #23804, #5412 ) ;
#23588 = CARTESIAN_POINT ( 'NONE',  ( 2.121777613921716821, 30.62783393162584389, -0.4070726844702514668 ) ) ;
#23589 = VERTEX_POINT ( 'NONE', #22903 ) ;
#23590 = CARTESIAN_POINT ( 'NONE',  ( 4.701602651720952153, 14.74110825330134844, 3.931159545749582040 ) ) ;
#23591 = CARTESIAN_POINT ( 'NONE',  ( -2.464088664829000130, 27.05663313895000144, 0.1453149127352000025 ) ) ;
#23592 = AXIS2_PLACEMENT_3D ( 'NONE', #5119, #15751, #4876 ) ;
#23593 = EDGE_CURVE ( 'NONE', #17322, #15241, #11781, .T. ) ;
#23594 = CARTESIAN_POINT ( 'NONE',  ( -24.50000000000000000, -8.081477262649000792, -6.807253044743999837 ) ) ;
#23595 = CARTESIAN_POINT ( 'NONE',  ( 2.426425728984999974, 26.63187716036000197, -0.3356153332445000470 ) ) ;
#23596 = CARTESIAN_POINT ( 'NONE',  ( 4.000000000000000000, 26.20000000000000284, -2.309401076759000304 ) ) ;
#23597 = ORIENTED_EDGE ( 'NONE', *, *, #15630, .T. ) ;
#23598 = FACE_OUTER_BOUND ( 'NONE', #3229, .T. ) ;
#23599 = EDGE_CURVE ( 'NONE', #19778, #15589, #23313, .T. ) ;
#23600 = CARTESIAN_POINT ( 'NONE',  ( 4.825047752666590029, 12.44037768847285363, -0.5059731828766852457 ) ) ;
#23601 = CARTESIAN_POINT ( 'NONE',  ( 24.21257416121859407, 4.458793670155209554, -8.532776386654354894 ) ) ;
#23602 = CARTESIAN_POINT ( 'NONE',  ( -21.35476253787999923, 9.219287007783998789, 0.000000000000000000 ) ) ;
#23603 = ORIENTED_EDGE ( 'NONE', *, *, #882, .F. ) ;
#23604 = CARTESIAN_POINT ( 'NONE',  ( -10.04281598263999875, 20.50000000000000000, 1.000000000000000000 ) ) ;
#23605 = CARTESIAN_POINT ( 'NONE',  ( 15.47718892131000068, -5.177634673800000975, -8.189908713891000502 ) ) ;
#23606 = CARTESIAN_POINT ( 'NONE',  ( 18.47504315980862444, 10.13530769844259360, -2.440014412375295816 ) ) ;
#23607 = ORIENTED_EDGE ( 'NONE', *, *, #1873, .T. ) ;
#23608 = EDGE_CURVE ( 'NONE', #19340, #4163, #9957, .T. ) ;
#23609 = CARTESIAN_POINT ( 'NONE',  ( -1.999167105995452998, 28.71666666666667211, -1.536366799937284089 ) ) ;
#23610 = CARTESIAN_POINT ( 'NONE',  ( 0.3885619843355000436, 29.77417815385999944, 2.502828369449000334 ) ) ;
#23611 = LINE ( 'NONE', #10659, #9275 ) ;
#23612 = DIRECTION ( 'NONE',  ( -1.000000000000000000, 0.000000000000000000, 0.000000000000000000 ) ) ;
#23613 = ORIENTED_EDGE ( 'NONE', *, *, #4698, .T. ) ;
#23614 = CARTESIAN_POINT ( 'NONE',  ( 0.000000000000000000, 22.00000000000000000, -4.549999999999999822 ) ) ;
#23615 = CARTESIAN_POINT ( 'NONE',  ( -24.50000000000292033, -11.08154813082897228, 5.806195610894957504 ) ) ;
#23616 = CARTESIAN_POINT ( 'NONE',  ( 30.87226923053214378, 27.01856778792605240, 2.673746900119611247 ) ) ;
#23617 = FACE_OUTER_BOUND ( 'NONE', #3516, .T. ) ;
#23618 = CARTESIAN_POINT ( 'NONE',  ( -1.236362846991004183, 26.50000008335574719, -2.171602059085420589 ) ) ;
#23619 = CARTESIAN_POINT ( 'NONE',  ( -2.818367767609784025, 24.55137445130671381, 2.991616928423203259 ) ) ;
#23620 = LINE ( 'NONE', #7251, #10418 ) ;
#23621 = CARTESIAN_POINT ( 'NONE',  ( 19.94399770046332421, 1.202189832516935564, 9.183084001584736811 ) ) ;
#23622 = ORIENTED_EDGE ( 'NONE', *, *, #14987, .T. ) ;
#23623 = LINE ( 'NONE', #15974, #21067 ) ;
#23624 = DIRECTION ( 'NONE',  ( -1.000000000000000000, 0.000000000000000000, 0.000000000000000000 ) ) ;
#23625 = VERTEX_POINT ( 'NONE', #4510 ) ;
#23626 = CARTESIAN_POINT ( 'NONE',  ( -0.3158523902254999904, 25.37040927195999984, -2.525508413827000087 ) ) ;
#23627 = EDGE_CURVE ( 'NONE', #14691, #14280, #4371, .T. ) ;
#23628 = CARTESIAN_POINT ( 'NONE',  ( 5.752994088155999108, 14.16261243406998993, 1.981461215821998190 ) ) ;
#23629 = CARTESIAN_POINT ( 'NONE',  ( 11.06626444616513005, -0.2510812432905764058, -12.49999588481644075 ) ) ;
#23630 = ADVANCED_FACE ( 'NONE', ( #6567 ), #13951, .F. ) ;
#23631 = CARTESIAN_POINT ( 'NONE',  ( 6.223219914810721676, 13.77310067638714663, -1.261352567770426480 ) ) ;
#23632 = DIRECTION ( 'NONE',  ( -0.5000000000000169864, 0.000000000000000000, 0.8660254037844289376 ) ) ;
#23633 =( NAMED_UNIT ( * ) SI_UNIT ( $, .STERADIAN. ) SOLID_ANGLE_UNIT ( ) );
#23634 = ORIENTED_EDGE ( 'NONE', *, *, #16504, .F. ) ;
#23635 = CARTESIAN_POINT ( 'NONE',  ( -18.03317485555000133, 9.527592921995999831, -4.015252424095000272 ) ) ;
#23636 = AXIS2_PLACEMENT_3D ( 'NONE', #19239, #9678, #11623 ) ;
#23637 = DIRECTION ( 'NONE',  ( -1.000000000000000000, 0.000000000000000000, 0.000000000000000000 ) ) ;
#23638 = ORIENTED_EDGE ( 'NONE', *, *, #6717, .F. ) ;
#23639 = EDGE_CURVE ( 'NONE', #17884, #6263, #13250, .T. ) ;
#23640 = CARTESIAN_POINT ( 'NONE',  ( -19.40498875207000040, -4.215398836441999642, 9.787615664903000834 ) ) ;
#23641 = ADVANCED_FACE ( 'NONE', ( #20940 ), #1663, .F. ) ;
#23642 = DIRECTION ( 'NONE',  ( -0.000000000000000000, 1.000000000000000000, 0.000000000000000000 ) ) ;
#23643 = CARTESIAN_POINT ( 'NONE',  ( 14.50354924558716796, 1.418337556017691181, -10.23477940919253548 ) ) ;
#23644 = DIRECTION ( 'NONE',  ( 0.000000000000000000, 0.000000000000000000, -1.000000000000000000 ) ) ;
#23645 = CARTESIAN_POINT ( 'NONE',  ( 23.75879881943000171, 10.74622900717000107, 3.476693416134999826 ) ) ;
#23646 = CARTESIAN_POINT ( 'NONE',  ( 2.067768348872000228, 29.65163254276000160, 0.6515505822407000602 ) ) ;
#23647 = CARTESIAN_POINT ( 'NONE',  ( 13.60029401354574219, 6.915711735797342108, -5.790824394749706450 ) ) ;
#23648 = CARTESIAN_POINT ( 'NONE',  ( -4.459918930441997276, 12.50682294446000142, -1.621453085808000516 ) ) ;
#23649 = VERTEX_POINT ( 'NONE', #20578 ) ;
#23650 = CARTESIAN_POINT ( 'NONE',  ( -1.911995322407668896, 26.28293724889640259, 1.064052824085054416 ) ) ;
#23651 = ORIENTED_EDGE ( 'NONE', *, *, #6288, .T. ) ;
#23652 = FACE_BOUND ( 'NONE', #3735, .T. ) ;
#23653 = CARTESIAN_POINT ( 'NONE',  ( 0.000000000000000000, 22.10000000618969906, 0.000000000000000000 ) ) ;
#23654 = ORIENTED_EDGE ( 'NONE', *, *, #477, .F. ) ;
#23655 = CARTESIAN_POINT ( 'NONE',  ( 11.32654380052867005, -12.11008572905893566, -4.024656720663734255 ) ) ;
#23656 = DIRECTION ( 'NONE',  ( -0.8206518066482797469, -0.5714285714285857187, 0.000000000000000000 ) ) ;
#23657 = CARTESIAN_POINT ( 'NONE',  ( 14.51266099164999979, 10.53307723766999970, -3.225898445907000145 ) ) ;
#23658 = ORIENTED_EDGE ( 'NONE', *, *, #19030, .F. ) ;
#23659 = CARTESIAN_POINT ( 'NONE',  ( -11.82901863877000004, 11.07399071560000081, 10.43874032931999984 ) ) ;
#23660 = CARTESIAN_POINT ( 'NONE',  ( 13.49999999999999822, 9.484469744014797143, -1.016853796975950575 ) ) ;
#23661 = CYLINDRICAL_SURFACE ( 'NONE', #21415, 1.500000000000001332 ) ;
#23662 = ORIENTED_EDGE ( 'NONE', *, *, #14508, .F. ) ;
#23663 = CARTESIAN_POINT ( 'NONE',  ( 22.26459748180845111, 5.667341905249820400, 8.925277597039414701 ) ) ;
#23664 = CARTESIAN_POINT ( 'NONE',  ( -2.693005968609320622, 26.46241504948188705, 3.063994432611676810 ) ) ;
#23665 = CARTESIAN_POINT ( 'NONE',  ( 15.91794248114183574, -9.831652891108184633, -3.269710195000794961 ) ) ;
#23666 = CARTESIAN_POINT ( 'NONE',  ( -16.82086276118999990, 1.975286977287000090, -10.89076854460999932 ) ) ;
#23667 = CONICAL_SURFACE ( 'NONE', #13213, 4.674999969225999585, 0.7853981633972997312 ) ;
#23668 = CARTESIAN_POINT ( 'NONE',  ( -0.8469014928486000571, 30.08331639939000013, -2.017769495180000483 ) ) ;
#23669 = PRODUCT_DEFINITION_CONTEXT ( 'detailed design', #22110, 'design' ) ;
#23670 = CARTESIAN_POINT ( 'NONE',  ( -15.75798294665000121, 9.136783202530001091, 3.374990494159999965 ) ) ;
#23671 = CARTESIAN_POINT ( 'NONE',  ( 0.6579082771927615703, 29.96447688474591331, -2.058286849431618659 ) ) ;
#23672 = ORIENTED_EDGE ( 'NONE', *, *, #4821, .F. ) ;
#23673 = CARTESIAN_POINT ( 'NONE',  ( 23.39997263175174425, -2.403873558705119429, 8.975496745306065449 ) ) ;
#23674 = CARTESIAN_POINT ( 'NONE',  ( 11.78693030656032725, 12.98156941793456376, -2.515258941385983160 ) ) ;
#23675 = CARTESIAN_POINT ( 'NONE',  ( 20.72484988667089212, 3.141094275043142314, 10.05519821595702901 ) ) ;
#23676 = DIRECTION ( 'NONE',  ( 0.000000000000000000, -1.000000000000000000, 0.000000000000000000 ) ) ;
#23677 = AXIS2_PLACEMENT_3D ( 'NONE', #3764, #1603, #23862 ) ;
#23678 = ORIENTED_EDGE ( 'NONE', *, *, #15166, .F. ) ;
#23679 = CARTESIAN_POINT ( 'NONE',  ( -12.50000000000000000, 6.992973968623999781, -5.709239639804999378 ) ) ;
#23680 = CARTESIAN_POINT ( 'NONE',  ( -14.25547544441000092, -7.466299210344000237, -11.77864653853000121 ) ) ;
#23681 = CARTESIAN_POINT ( 'NONE',  ( 4.548030535609999703, 12.31234507743998563, -1.688239928504997600 ) ) ;
#23682 = ORIENTED_EDGE ( 'NONE', *, *, #4667, .F. ) ;
#23683 = CARTESIAN_POINT ( 'NONE',  ( 16.43793875730999687, -4.200504661774999704, 8.191206307881000015 ) ) ;
#23684 = ORIENTED_EDGE ( 'NONE', *, *, #8029, .F. ) ;
#23685 = AXIS2_PLACEMENT_3D ( 'NONE', #141, #7533, #13338 ) ;
#23686 = CARTESIAN_POINT ( 'NONE',  ( -1.554837348280936338, 26.73126847659393235, -1.516119970887816359 ) ) ;
#23687 = CARTESIAN_POINT ( 'NONE',  ( -14.49863740500227216, 0.5184489068879251095, -12.49996363569464819 ) ) ;
#23688 = ORIENTED_EDGE ( 'NONE', *, *, #10769, .T. ) ;
#23689 = DIRECTION ( 'NONE',  ( -0.1592000000000055038, 0.9872463522343337683, 0.000000000000000000 ) ) ;
#23690 = CARTESIAN_POINT ( 'NONE',  ( -19.99227829421999658, -4.688870380650000058, 9.502835446995000268 ) ) ;
#23691 = CARTESIAN_POINT ( 'NONE',  ( 0.000000000000000000, 9.000000000000000000, 0.000000000000000000 ) ) ;
#23692 = CARTESIAN_POINT ( 'NONE',  ( 18.37479166666664909, -9.142815082014921657, -1.196664747960725084 ) ) ;
#23693 = CARTESIAN_POINT ( 'NONE',  ( -24.37031988197636423, 2.803527235482467628, -10.22615976150734340 ) ) ;
#23694 = CARTESIAN_POINT ( 'NONE',  ( 1.988574678778234794, 26.55190665974927100, 0.8727035924344519469 ) ) ;
#23695 = DIRECTION ( 'NONE',  ( -1.000000000000000000, 0.000000000000000000, 0.000000000000000000 ) ) ;
#23696 = ADVANCED_FACE ( 'NONE', ( #221 ), #5713, .F. ) ;
#23697 = CARTESIAN_POINT ( 'NONE',  ( -1.350914310362234527, 29.97444252552742583, 3.838851412777819938 ) ) ;
#23698 = ORIENTED_EDGE ( 'NONE', *, *, #9271, .F. ) ;
#23699 = DIRECTION ( 'NONE',  ( 0.000000000000000000, -0.9925668416490733836, -0.1217007183987965646 ) ) ;
#23700 = DIRECTION ( 'NONE',  ( -1.000000000000000000, 0.000000000000000000, 0.000000000000000000 ) ) ;
#23701 = CARTESIAN_POINT ( 'NONE',  ( 1.996953125041000199, 26.56913313895000073, 1.450871306011999984 ) ) ;
#23702 = AXIS2_PLACEMENT_3D ( 'NONE', #14189, #12616, #2933 ) ;
#23703 = CARTESIAN_POINT ( 'NONE',  ( -2.000256872717999901, 28.45364211381999908, 1.120191590154000050 ) ) ;
#23704 = CARTESIAN_POINT ( 'NONE',  ( 4.492058920961061297, 12.31709606397016898, 1.815161732821968021 ) ) ;
#23705 = ORIENTED_EDGE ( 'NONE', *, *, #15985, .F. ) ;
#23706 = CARTESIAN_POINT ( 'NONE',  ( 0.000000000000000000, 24.40000007355299871, 0.000000000000000000 ) ) ;
#23707 = CARTESIAN_POINT ( 'NONE',  ( 0.3616284121818696962, 11.48838882713601883, -4.797856110140303443 ) ) ;
#23708 = EDGE_CURVE ( 'NONE', #12888, #2468, #12582, .T. ) ;
#23709 = CARTESIAN_POINT ( 'NONE',  ( -10.33761176360648371, 15.67664585749226802, 1.227329692040328490 ) ) ;
#23710 = CARTESIAN_POINT ( 'NONE',  ( 2.241434001307105017, 30.45310926007345032, -0.4064658644085604733 ) ) ;
#23711 = VERTEX_POINT ( 'NONE', #492 ) ;
#23712 = FACE_OUTER_BOUND ( 'NONE', #9427, .T. ) ;
#23713 = FACE_OUTER_BOUND ( 'NONE', #13600, .T. ) ;
#23714 = AXIS2_PLACEMENT_3D ( 'NONE', #10256, #8567, #799 ) ;
#23715 = CARTESIAN_POINT ( 'NONE',  ( 14.38031392131000175, 9.076879665875999592, 3.306787424407999776 ) ) ;
#23716 = CARTESIAN_POINT ( 'NONE',  ( 18.45488575664959896, 9.937485657898088576, -3.138395590753138009 ) ) ;
#23717 = UNCERTAINTY_MEASURE_WITH_UNIT (LENGTH_MEASURE( 1.000000000000000082E-05 ), #1957, 'distance_accuracy_value', 'NONE');
#23718 = CARTESIAN_POINT ( 'NONE',  ( 2.434931691670791487, 29.40086340285667887, 0.6543697108981911814 ) ) ;
#23719 = CARTESIAN_POINT ( 'NONE',  ( 0.8875055740816000238, 29.99964212565999944, -2.167090567999999884 ) ) ;
#23720 = CARTESIAN_POINT ( 'NONE',  ( 18.71296080085999947, 8.147654916100000477, 8.033579312641000669 ) ) ;
#23721 = CARTESIAN_POINT ( 'NONE',  ( 13.50000000000000178, -9.655853724928261883, 1.323126653348174697 ) ) ;
#23722 = B_SPLINE_CURVE_WITH_KNOTS ( 'NONE', 3,
 ( #16272, #15904, #12651, #23664, #19807, #7075, #14459, #17624, #8420, #15788 ),
 .UNSPECIFIED., .F., .F.,
 ( 4, 1, 1, 2, 2, 4 ),
 ( 0.000000000000000000, 0.2500000000000001665, 0.3750000000000001665, 0.4375000000000000555, 0.4999999999999999445, 1.000000000000000000 ),
 .UNSPECIFIED. ) ;
#23723 = ORIENTED_EDGE ( 'NONE', *, *, #13824, .T. ) ;
#23724 = CARTESIAN_POINT ( 'NONE',  ( -24.50000000000000000, 10.82531754731000007, 6.250000000000000000 ) ) ;
#23725 = CARTESIAN_POINT ( 'NONE',  ( 23.93688783760000049, 6.590125990732999206, -8.595340802195000407 ) ) ;
#23726 = ADVANCED_FACE ( 'NONE', ( #6432 ), #7456, .T. ) ;
#23727 = CARTESIAN_POINT ( 'NONE',  ( 1.259047450927267553, 29.06666666666666288, 2.184465970885633990 ) ) ;
#23728 = DIRECTION ( 'NONE',  ( -0.000000000000000000, 0.8660254037844288266, 0.5000000000000169864 ) ) ;
#23729 = CARTESIAN_POINT ( 'NONE',  ( -4.071056736052401703, 13.78562280736089107, 4.868570922598909334 ) ) ;
#23730 = CARTESIAN_POINT ( 'NONE',  ( 3.799177505463000593, 12.12209995490999326, 3.177317162311001031 ) ) ;
#23731 = CARTESIAN_POINT ( 'NONE',  ( 21.91677564524291455, 36.61664399927605018, -6.000000000000000000 ) ) ;
#23732 = ORIENTED_EDGE ( 'NONE', *, *, #13487, .T. ) ;
#23733 = FACE_OUTER_BOUND ( 'NONE', #4146, .T. ) ;
#23734 = DIRECTION ( 'NONE',  ( -1.000000000000000000, 0.000000000000000000, 0.000000000000000000 ) ) ;
#23735 = EDGE_LOOP ( 'NONE', ( #2938, #16429, #2927 ) ) ;
#23736 = CARTESIAN_POINT ( 'NONE',  ( -1.739863589215999928, 24.46283721557000135, -1.282156090217000166 ) ) ;
#23737 = CARTESIAN_POINT ( 'NONE',  ( 0.000000000000000000, 26.50000000000000355, 0.000000000000000000 ) ) ;
#23738 = EDGE_CURVE ( 'NONE', #16256, #8876, #21846, .T. ) ;
#23739 = CARTESIAN_POINT ( 'NONE',  ( 11.66614181937909578, -3.921044720226404046, -12.49992990204019527 ) ) ;
#23740 = CARTESIAN_POINT ( 'NONE',  ( 6.224373531547387373, 13.76762753968859165, -1.282219680938367690 ) ) ;
#23741 = CARTESIAN_POINT ( 'NONE',  ( 0.000000000000000000, 24.50000000000000000, 0.000000000000000000 ) ) ;
#23743 = AXIS2_PLACEMENT_3D ( 'NONE', #2873, #12321, #5062 ) ;
#23742 = DIRECTION ( 'NONE',  ( 0.000000000000000000, -1.000000000000000000, 0.000000000000000000 ) ) ;
#23744 = ORIENTED_EDGE ( 'NONE', *, *, #23419, .F. ) ;
#23745 = CARTESIAN_POINT ( 'NONE',  ( 0.000000000000000000, 18.00000000000000000, -2.899999999999999911 ) ) ;
#23746 = FACE_OUTER_BOUND ( 'NONE', #4173, .T. ) ;
#23747 = EDGE_CURVE ( 'NONE', #12555, #14083, #4501, .T. ) ;
#23748 = CARTESIAN_POINT ( 'NONE',  ( -3.999878274658704935, 24.63336607547242707, 1.519686587934140576 ) ) ;
#23749 = ORIENTED_EDGE ( 'NONE', *, *, #23015, .T. ) ;
#23750 = CARTESIAN_POINT ( 'NONE',  ( -10.83930303495209380, 15.36257445830826285, -1.684799336714881468 ) ) ;
#23751 = CARTESIAN_POINT ( 'NONE',  ( -1.953659355438999823, 23.74463359794000183, 0.8845564191319000846 ) ) ;
#23752 = CARTESIAN_POINT ( 'NONE',  ( 14.42261690652483352, -1.401882518806423228, -10.22223842188914311 ) ) ;
#23753 = CARTESIAN_POINT ( 'NONE',  ( 8.124934037954998800, 0.000000000000000000, 0.000000000000000000 ) ) ;
#23754 = CARTESIAN_POINT ( 'NONE',  ( 21.15221597181999869, -10.99634298136000154, -2.244525743171999821 ) ) ;
#23755 = ADVANCED_FACE ( 'NONE', ( #11892 ), #10580, .F. ) ;
#23756 = CARTESIAN_POINT ( 'NONE',  ( -0.9609966757344999833, 29.14897034355999850, -1.943365538522000113 ) ) ;
#23757 = CARTESIAN_POINT ( 'NONE',  ( 13.80186061669689224, 9.025291446785679739, 0.005808137674083918567 ) ) ;
#23758 = EDGE_CURVE ( 'NONE', #9908, #19829, #4779, .T. ) ;
#23759 = CARTESIAN_POINT ( 'NONE',  ( -1.421060907519000382, 11.74865550866998731, -4.622470049807997583 ) ) ;
#23760 = DIRECTION ( 'NONE',  ( -1.000000000000000000, 0.000000000000000000, 0.000000000000000000 ) ) ;
#23761 = ORIENTED_EDGE ( 'NONE', *, *, #168, .F. ) ;
#23762 = CONICAL_SURFACE ( 'NONE', #13304, 14.15464499511999996, 0.6126053401530057174 ) ;
#23763 = CARTESIAN_POINT ( 'NONE',  ( -2.000000000000000000, 28.00000000000000000, 3.464101615137999968 ) ) ;
#23764 = ORIENTED_EDGE ( 'NONE', *, *, #19645, .F. ) ;
#23765 = FACE_OUTER_BOUND ( 'NONE', #10161, .T. ) ;
#23766 = DIRECTION ( 'NONE',  ( 1.000000000000000000, 0.000000000000000000, 0.000000000000000000 ) ) ;
#23767 = EDGE_CURVE ( 'NONE', #13042, #20998, #11655, .T. ) ;
#23768 = CARTESIAN_POINT ( 'NONE',  ( 21.64462270046331938, 4.646871317838020765, 8.062138474834723567 ) ) ;
#23769 = EDGE_CURVE ( 'NONE', #23810, #9862, #6192, .T. ) ;
#23770 = CARTESIAN_POINT ( 'NONE',  ( 13.42995560457999993, -6.779495263956999196, 8.645408472313999226 ) ) ;
#23771 = ORIENTED_EDGE ( 'NONE', *, *, #15594, .T. ) ;
#23772 = CIRCLE ( 'NONE', #9085, 0.09999999999999939493 ) ;
#23773 = CARTESIAN_POINT ( 'NONE',  ( -10.61452256585000065, 4.516066062789000135, -14.16555620123000026 ) ) ;
#23774 = CARTESIAN_POINT ( 'NONE',  ( 13.49999999999999822, 6.231970360783858354, -6.769108791265136205 ) ) ;
#23775 = DIRECTION ( 'NONE',  ( 0.7071067811905932254, -0.7071067811824932603, 1.099460906822990477E-07 ) ) ;
#23776 = EDGE_LOOP ( 'NONE', ( #3585, #6770, #11171, #9166, #22182, #10850 ) ) ;
#23777 = CARTESIAN_POINT ( 'NONE',  ( 21.97045161944091873, 10.72494003805814344, -0.1196986000478276607 ) ) ;
#23778 = LINE ( 'NONE', #9250, #10285 ) ;
#23779 = CARTESIAN_POINT ( 'NONE',  ( 16.10619618340015791, -5.817247716720235218, -8.575685592426966153 ) ) ;
#23780 = CARTESIAN_POINT ( 'NONE',  ( -18.26616928144000340, 11.03552772663999981, -1.267153208245000107 ) ) ;
#23781 = CARTESIAN_POINT ( 'NONE',  ( -1.947074432796000121, 29.48947843130000379, 1.303234819910000120 ) ) ;
#23782 = VECTOR ( 'NONE', #16831, 1000.000000000000000 ) ;
#23783 = CARTESIAN_POINT ( 'NONE',  ( -18.73722805020999616, -7.945584595330000610, 4.815966472443999891 ) ) ;
#23784 = CARTESIAN_POINT ( 'NONE',  ( 2.135618988582168143, 29.82286535022900864, -0.3226676719785777081 ) ) ;
#23785 = EDGE_LOOP ( 'NONE', ( #12083, #12521, #9546, #22915, #10344 ) ) ;
#23786 = CARTESIAN_POINT ( 'NONE',  ( 23.24887628969795372, 2.425622639895666399, 9.025022120430918449 ) ) ;
#23787 = CARTESIAN_POINT ( 'NONE',  ( 20.18575559708055778, 8.684556385100460574, -5.939556492853414582 ) ) ;
#23788 = CARTESIAN_POINT ( 'NONE',  ( -0.8574870095143278803, 23.63963447597672030, -1.960294260298593549 ) ) ;
#23789 = VERTEX_POINT ( 'NONE', #4381 ) ;
#23790 = CARTESIAN_POINT ( 'NONE',  ( 12.50898179946000077, 6.466848119989000665, 12.35567989459000060 ) ) ;
#23791 = CYLINDRICAL_SURFACE ( 'NONE', #13130, 13.93375672974000068 ) ;
#23792 = CARTESIAN_POINT ( 'NONE',  ( 3.211718233129003508, 11.87833580068998351, -3.657054441831002034 ) ) ;
#23793 = VERTEX_POINT ( 'NONE', #11773 ) ;
#23794 = CARTESIAN_POINT ( 'NONE',  ( 4.750000000000000000, 20.10000000000000142, 0.000000000000000000 ) ) ;
#23795 = VERTEX_POINT ( 'NONE', #2557 ) ;
#23796 = AXIS2_PLACEMENT_3D ( 'NONE', #5561, #18636, #5448 ) ;
#23797 = CARTESIAN_POINT ( 'NONE',  ( -2.434931691670786602, 28.26753006952333536, 0.6543697108982093891 ) ) ;
#23798 = CONTEXT_DEPENDENT_SHAPE_REPRESENTATION ( #12221, #888 ) ;
#23799 = CARTESIAN_POINT ( 'NONE',  ( 2.500000000000000000, 30.00000000000000000, 0.000000000000000000 ) ) ;
#23800 = ORIENTED_EDGE ( 'NONE', *, *, #8515, .F. ) ;
#23801 = CARTESIAN_POINT ( 'NONE',  ( -15.42147087121333371, -1.186998013042046773, 9.067027049713395570 ) ) ;
#23802 = APPLICATION_CONTEXT ( 'automotive_design' ) ;
#23803 = CARTESIAN_POINT ( 'NONE',  ( -20.10087239461999786, -8.560891429069998892, 5.321486511249999829 ) ) ;
#23804 = DIRECTION ( 'NONE',  ( 0.000000000000000000, 1.000000000000000000, 0.000000000000000000 ) ) ;
#23805 = CARTESIAN_POINT ( 'NONE',  ( -4.771218631688002532, 13.11106448824000026, -5.073972735316997884 ) ) ;
#23806 = CARTESIAN_POINT ( 'NONE',  ( -23.21223922333086875, -9.596433927533320585, 4.441285397424103998 ) ) ;
#23807 = CARTESIAN_POINT ( 'NONE',  ( -1.955724675740084795, 26.26076676662178855, 0.9180910909140133080 ) ) ;
#23808 = CARTESIAN_POINT ( 'NONE',  ( -5.824604845557002974, 16.40175155375999339, 2.021265510678000421 ) ) ;
#23809 = CONICAL_SURFACE ( 'NONE', #199, 9.157130689899000586, 0.02565634000431304615 ) ;
#23810 = VERTEX_POINT ( 'NONE', #21706 ) ;
#23811 = CARTESIAN_POINT ( 'NONE',  ( -17.12209587121333954, -4.588422834071612222, 7.960729490015661547 ) ) ;
#23812 = CARTESIAN_POINT ( 'NONE',  ( 3.779214145209469855, 14.37913731383023297, 4.820907688989376716 ) ) ;
#23813 = CARTESIAN_POINT ( 'NONE',  ( 14.77567797042977027, -6.635935015099072132, 6.230487974134251594 ) ) ;
#23814 = CARTESIAN_POINT ( 'NONE',  ( 5.819228265851155157, 14.45505663675167796, -1.911080848660286158 ) ) ;
#23815 = CARTESIAN_POINT ( 'NONE',  ( -1.552970335759000120, 27.13771896306000286, 1.679993844339999987 ) ) ;
#23816 = DIRECTION ( 'NONE',  ( 0.000000000000000000, -1.000000000000000000, -9.414809210018000201E-11 ) ) ;
#23817 = ORIENTED_EDGE ( 'NONE', *, *, #12889, .T. ) ;
#23818 = CARTESIAN_POINT ( 'NONE',  ( -2.695181268941200692, 11.78983089400772855, -4.000416410329833639 ) ) ;
#23819 = CARTESIAN_POINT ( 'NONE',  ( 0.000000000000000000, 24.80000000000000426, -4.618802153517000519 ) ) ;
#23820 = CARTESIAN_POINT ( 'NONE',  ( 2.149044184505269683, 28.87331377689345757, -0.7555511948961874946 ) ) ;
#23821 = ORIENTED_EDGE ( 'NONE', *, *, #5402, .T. ) ;
#23822 = ADVANCED_FACE ( 'NONE', ( #21818 ), #10949, .F. ) ;
#23823 = FACE_OUTER_BOUND ( 'NONE', #20989, .T. ) ;
#23824 = CARTESIAN_POINT ( 'NONE',  ( -16.17730420454665463, 5.584121353372251129, -7.266021601655057616 ) ) ;
#23825 = VECTOR ( 'NONE', #15501, 1000.000000000000000 ) ;
#23826 = VECTOR ( 'NONE', #9510, 1000.000000000000000 ) ;
#23827 = CARTESIAN_POINT ( 'NONE',  ( 11.52843892131000025, -9.307182416847998851, 0.9706197651944000748 ) ) ;
#23828 = CARTESIAN_POINT ( 'NONE',  ( 18.45819154983377786, 9.973350390120506503, -3.023520947057698915 ) ) ;
#23829 = CARTESIAN_POINT ( 'NONE',  ( 1.999167105995457216, 29.35086340285667106, 1.536366799937278760 ) ) ;
#23830 = CARTESIAN_POINT ( 'NONE',  ( 0.4270404191337999755, 28.76915224701999918, 2.107898681223999926 ) ) ;
#23831 = LINE ( 'NONE', #13048, #23238 ) ;
#23832 = CARTESIAN_POINT ( 'NONE',  ( 0.000000000000000000, 12.90000000000000036, 0.000000000000000000 ) ) ;
#23833 = ORIENTED_EDGE ( 'NONE', *, *, #21015, .F. ) ;
#23834 = CARTESIAN_POINT ( 'NONE',  ( -8.250000000000000000, 22.87500000000000000, -6.000000000000000000 ) ) ;
#23835 = CARTESIAN_POINT ( 'NONE',  ( 22.78033775462999699, -7.550126252767999979, 8.445756667117999328 ) ) ;
#23836 = EDGE_CURVE ( 'NONE', #10709, #11527, #6215, .T. ) ;
#23837 = CARTESIAN_POINT ( 'NONE',  ( -24.00397000733149966, 1.618184422371759856, 9.698553049397601100 ) ) ;
#23838 = VECTOR ( 'NONE', #10731, 1000.000000000000000 ) ;
#23839 = CARTESIAN_POINT ( 'NONE',  ( 13.86248033612164754, -10.18903838342320611, -1.816066799785956087 ) ) ;
#23840 = LINE ( 'NONE', #11132, #19179 ) ;
#23841 = CARTESIAN_POINT ( 'NONE',  ( 4.103561096572000189, 12.21754528531001149, 2.770293696547999840 ) ) ;
#23842 = CARTESIAN_POINT ( 'NONE',  ( -0.5478863511337975778, 29.23652871585738922, -2.091076401733357404 ) ) ;
#23843 = CARTESIAN_POINT ( 'NONE',  ( -12.25000000000000000, 11.84440073488268652, -9.209314101129749019 ) ) ;
#23844 = ORIENTED_EDGE ( 'NONE', *, *, #1261, .F. ) ;
#23845 = B_SPLINE_CURVE_WITH_KNOTS ( 'NONE', 3,
 ( #260, #13828, #8021, #4389, #17719, #19534, #989, #6439 ),
 .UNSPECIFIED., .F., .F.,
 ( 4, 2, 2, 4 ),
 ( 0.000000000000000000, 0.2500000000000002776, 0.5000000000000005551, 1.000000000000000000 ),
 .UNSPECIFIED. ) ;
#23846 = AXIS2_PLACEMENT_3D ( 'NONE', #14336, #17970, #5136 ) ;
#23847 = CARTESIAN_POINT ( 'NONE',  ( 0.3463667137627760018, 24.70780860099773690, -4.418706525551467479 ) ) ;
#23848 = ORIENTED_EDGE ( 'NONE', *, *, #14968, .T. ) ;
#23849 = CARTESIAN_POINT ( 'NONE',  ( -2.014261560068999923, 23.69646414078999896, -0.7835128413787000312 ) ) ;
#23850 = CARTESIAN_POINT ( 'NONE',  ( 6.140636424933997972, 13.62023824745998901, 2.542827786053999617 ) ) ;
#23851 = CARTESIAN_POINT ( 'NONE',  ( 11.78924557931654249, -4.312980057965595471, -12.49999285599341547 ) ) ;
#23852 = DIRECTION ( 'NONE',  ( 0.000000000000000000, 8.881784197001252323E-16, 1.000000000000000000 ) ) ;
#23853 = CARTESIAN_POINT ( 'NONE',  ( -1.536366799937290084, 27.88333333333333641, -1.999167105995448113 ) ) ;
#23854 = CARTESIAN_POINT ( 'NONE',  ( 18.60131424931000055, 8.248882947719001990, 6.955037127929000640 ) ) ;
#23855 = EDGE_CURVE ( 'NONE', #1933, #17483, #3299, .T. ) ;
#23856 = DIRECTION ( 'NONE',  ( 0.000000000000000000, 0.000000000000000000, 1.000000000000000000 ) ) ;
#23857 = CONICAL_SURFACE ( 'NONE', #17683, 2.849999992212000066, 0.7853981633972997312 ) ;
#23858 = EDGE_LOOP ( 'NONE', ( #20426, #14976, #12732, #8172 ) ) ;
#23859 = CARTESIAN_POINT ( 'NONE',  ( -18.80493816619999947, -6.461643014194000223, 6.332623921217999552 ) ) ;
#23860 = CARTESIAN_POINT ( 'NONE',  ( 4.000000000000000000, 29.99999999999999645, 0.1857058784358717463 ) ) ;
#23861 = CIRCLE ( 'NONE', #13411, 1.500000000000001332 ) ;
#23862 = DIRECTION ( 'NONE',  ( 0.000000000000000000, 0.9981468999026679167, -0.06085035919937799298 ) ) ;
#23863 = ORIENTED_EDGE ( 'NONE', *, *, #16439, .T. ) ;
#23864 = CARTESIAN_POINT ( 'NONE',  ( -10.51126211288548795, 15.52477961147895158, -1.382190245016840846 ) ) ;
#23865 = CARTESIAN_POINT ( 'NONE',  ( 0.5583575531182999319, 24.25696251314999685, -2.070647963877000119 ) ) ;
#23866 = CARTESIAN_POINT ( 'NONE',  ( 14.52769910616910032, 2.258345615986147248, -10.08167035404599687 ) ) ;
#23867 = CARTESIAN_POINT ( 'NONE',  ( -18.25584587121333868, -2.392196265530771360, -8.901927720310109038 ) ) ;
#23868 = CARTESIAN_POINT ( 'NONE',  ( 18.97390937112000131, 0.006297815236294000002, 10.66796791185999993 ) ) ;
#23869 = CARTESIAN_POINT ( 'NONE',  ( -24.50000000000000000, 3.293267271483000247, -9.759323269498999309 ) ) ;
#23870 = ADVANCED_FACE ( 'NONE', ( #6795 ), #2829, .F. ) ;
#23871 = CARTESIAN_POINT ( 'NONE',  ( 13.79933150931701213, 9.025147458263377942, -0.07313042455966387023 ) ) ;
#23872 = CARTESIAN_POINT ( 'NONE',  ( -6.406436833942142250, 15.54626959098088612, -1.355418181164619762 ) ) ;
#23873 = CARTESIAN_POINT ( 'NONE',  ( -22.07280420454664949, -7.387003317728245477, -5.677096218463232091 ) ) ;
#23874 = EDGE_LOOP ( 'NONE', ( #17371, #3955, #12492, #13932, #11355, #5462, #21449, #3623, #20244, #756, #16895, #3415 ) ) ;
#23875 = CARTESIAN_POINT ( 'NONE',  ( -14.79391872048465295, -6.742496754366980483, -6.069009251390668602 ) ) ;
#23876 = CARTESIAN_POINT ( 'NONE',  ( -7.834000000000000519, 1.320585629393000037E-14, 0.000000000000000000 ) ) ;
#23877 = EDGE_CURVE ( 'NONE', #14911, #17463, #21587, .T. ) ;
#23878 = ORIENTED_EDGE ( 'NONE', *, *, #4369, .T. ) ;
#23879 = DIRECTION ( 'NONE',  ( 0.000000000000000000, 0.000000000000000000, -1.000000000000000000 ) ) ;
#23880 = CARTESIAN_POINT ( 'NONE',  ( 16.82533333333332237, -4.584587517879673335, -7.954075159630586533 ) ) ;
#23881 = CIRCLE ( 'NONE', #5329, 10.69999999999999929 ) ;
#23882 = FACE_OUTER_BOUND ( 'NONE', #11870, .T. ) ;
#23883 = B_SPLINE_CURVE_WITH_KNOTS ( 'NONE', 3,
 ( #12708, #1678, #23718, #1798, #23829, #3619, #20443, #3731, #18506, #18625, #1574, #87, #10780, #9067, #9305, #7359, #11001, #13046 ),
 .UNSPECIFIED., .F., .F.,
 ( 4, 2, 2, 2, 2, 2, 2, 2, 4 ),
 ( 0.000000000000000000, 0.1250000000000000000, 0.2500000000000000000, 0.3750000000000000000, 0.5000000000000000000, 0.6250000000000000000, 0.7500000000000000000, 0.8750000000000000000, 1.000000000000000000 ),
 .UNSPECIFIED. ) ;
#23884 = CARTESIAN_POINT ( 'NONE',  ( 15.56153707775999884, -10.50595843275999997, 3.407448292006999946 ) ) ;
#23885 = CARTESIAN_POINT ( 'NONE',  ( -14.36292368913682793, 3.214461816234695846, 9.839097687039936702 ) ) ;
#23886 = EDGE_CURVE ( 'NONE', #18634, #4204, #1231, .T. ) ;
#23887 = CARTESIAN_POINT ( 'NONE',  ( -0.3657850755361999884, 27.66212896667000010, 2.644546391786999795 ) ) ;
#23888 = EDGE_CURVE ( 'NONE', #10478, #22015, #14538, .T. ) ;
#23889 = VERTEX_POINT ( 'NONE', #5117 ) ;
#23890 = CARTESIAN_POINT ( 'NONE',  ( -9.494475065846000206, -14.25618727434000022, -4.221251427306000004 ) ) ;
#23891 = CARTESIAN_POINT ( 'NONE',  ( 13.50000000000000355, 7.849402262525473795, -4.941025682226755755 ) ) ;
#23892 = CARTESIAN_POINT ( 'NONE',  ( -2.899999999999999911, 19.00000000000000000, 0.000000000000000000 ) ) ;
#23893 = ORIENTED_EDGE ( 'NONE', *, *, #11060, .T. ) ;
#23894 = CARTESIAN_POINT ( 'NONE',  ( 22.41167041299115681, 0.6016933124379368891, 10.56272183056112368 ) ) ;
#23895 = CARTESIAN_POINT ( 'NONE',  ( 24.50000000000000000, 10.82531754731000007, -6.250000000000000000 ) ) ;
#23896 = CARTESIAN_POINT ( 'NONE',  ( 15.96138423613740365, -9.219108122161413732, -4.736901002440107256 ) ) ;
#23897 = VECTOR ( 'NONE', #4073, 1000.000000000000000 ) ;
#23898 = CARTESIAN_POINT ( 'NONE',  ( -17.14814767310999599, -4.781802597067000171, -9.992171950030998673 ) ) ;
#23899 = CARTESIAN_POINT ( 'NONE',  ( 2.047977397348999862, 30.58687554411000065, 0.7709893512285000972 ) ) ;
#23900 = EDGE_CURVE ( 'NONE', #11139, #6021, #1108, .T. ) ;
#23901 = CARTESIAN_POINT ( 'NONE',  ( -4.000000142211483478, 28.05137445130720408, -0.9449696197475782045 ) ) ;
#23902 = AXIS2_PLACEMENT_3D ( 'NONE', #11873, #19008, #21196 ) ;
#23903 = CARTESIAN_POINT ( 'NONE',  ( 2.137288283767348585, 29.82219721339723151, -0.3113321526725940647 ) ) ;
#23904 = ORIENTED_EDGE ( 'NONE', *, *, #6869, .T. ) ;
#23905 = CARTESIAN_POINT ( 'NONE',  ( -0.6999264713064999865, 23.99113176564999961, 2.066154116230000337 ) ) ;
#23906 = CARTESIAN_POINT ( 'NONE',  ( 20.80997003765781983, 0.08280392278151330054, 10.53160635407974155 ) ) ;
#23907 = CARTESIAN_POINT ( 'NONE',  ( -1.005978889223114070, 23.62285964557008100, -1.869535163937288358 ) ) ;
#23908 = ORIENTED_EDGE ( 'NONE', *, *, #4350, .T. ) ;
#23909 = CARTESIAN_POINT ( 'NONE',  ( 12.49102043339000012, 6.966815666558000331, 12.06702349699999921 ) ) ;
#23910 = CARTESIAN_POINT ( 'NONE',  ( -5.966156734610001955, 14.84369745517001249, 4.200616803647995390 ) ) ;
#23911 = CARTESIAN_POINT ( 'NONE',  ( 0.3761184368515001486, 11.43848625460998214, -4.857791548063001841 ) ) ;
#23912 = ORIENTED_EDGE ( 'NONE', *, *, #23769, .T. ) ;
#23913 = EDGE_CURVE ( 'NONE', #18102, #4867, #8509, .T. ) ;
#23914 = CARTESIAN_POINT ( 'NONE',  ( 13.36668875730999950, -6.148145076040000490, -6.742444596879999530 ) ) ;
#23915 = EDGE_CURVE ( 'NONE', #14322, #5160, #15732, .T. ) ;
#23916 = ORIENTED_EDGE ( 'NONE', *, *, #3293, .F. ) ;
#23917 = CARTESIAN_POINT ( 'NONE',  ( -2.500000000000000000, 28.23419673618999681, 0.000000000000000000 ) ) ;
#23918 = CARTESIAN_POINT ( 'NONE',  ( -14.49454881829679920, 0.9069790026173082387, -12.49996723895875839 ) ) ;
#23919 = CONICAL_SURFACE ( 'NONE', #13471, 13.23032192316000000, 1.093540295016705466 ) ;
#23920 = ORIENTED_EDGE ( 'NONE', *, *, #1992, .T. ) ;
#23921 = CARTESIAN_POINT ( 'NONE',  ( 22.66499770046333495, -1.211330063708917493, -9.252910224394478078 ) ) ;
#23922 = VECTOR ( 'NONE', #6020, 1000.000000000000000 ) ;
#23923 = PRESENTATION_LAYER_ASSIGNMENT (  '', '', ( #8060 ) ) ;
#23924 = CARTESIAN_POINT ( 'NONE',  ( -24.43671288875999892, 10.10651051612000018, 1.358723590744000065 ) ) ;
#23925 = CARTESIAN_POINT ( 'NONE',  ( -15.35503366218999943, 4.356420647583999717, 8.699100579126000099 ) ) ;
#23927 = EDGE_CURVE ( 'NONE', #2037, #3147, #15956, .T. ) ;
#23926 = CARTESIAN_POINT ( 'NONE',  ( -5.606472695148997154, 15.09370601804999623, -2.790885761882998750 ) ) ;
#23928 = EDGE_CURVE ( 'NONE', #22015, #2993, #19875, .T. ) ;
#23929 = CARTESIAN_POINT ( 'NONE',  ( -24.13870375024561454, 9.298829860497594524, -5.090628969465328169 ) ) ;
#23930 = CARTESIAN_POINT ( 'NONE',  ( 1.519660212291651602, 27.50594812747459983, -1.553771826035092340 ) ) ;
#23931 = CIRCLE ( 'NONE', #3451, 7.500000000000000000 ) ;
#23932 = DIRECTION ( 'NONE',  ( -0.000000000000000000, 0.5000000000000169864, 0.8660254037844288266 ) ) ;
#23933 = CARTESIAN_POINT ( 'NONE',  ( 1.358166937795349138, 30.71719867068216203, -1.679610467239872840 ) ) ;
#23934 = VERTEX_POINT ( 'NONE', #10805 ) ;
#23935 = CARTESIAN_POINT ( 'NONE',  ( 4.230504193311618977, 14.54539643883826372, 4.442872086443444779 ) ) ;
#23936 = CARTESIAN_POINT ( 'NONE',  ( 4.698364960988029360, 13.53628448261239470, -5.010774751729513810 ) ) ;
#23937 = CIRCLE ( 'NONE', #13486, 3.000000000000000000 ) ;
#23938 = CARTESIAN_POINT ( 'NONE',  ( -24.31263779340282483, -2.333065073542751833, -10.34449948205211633 ) ) ;
#23939 = CARTESIAN_POINT ( 'NONE',  ( 0.4306175354955999457, 26.43687716036000168, 2.411379030285999647 ) ) ;
#23940 = CARTESIAN_POINT ( 'NONE',  ( -2.123863125265573526, 30.86865349149609017, 0.1785559413447701804 ) ) ;
#23941 = CARTESIAN_POINT ( 'NONE',  ( 3.525966305170764148, 12.00356175602403930, 3.304555447279709401 ) ) ;
#23942 = ORIENTED_EDGE ( 'NONE', *, *, #17403, .T. ) ;
#23943 = B_SPLINE_CURVE_WITH_KNOTS ( 'NONE', 3,
 ( #15953, #17918, #12583, #12700, #3266, #23227, #16076, #14035, #21428, #4842, #19968, #19850, #10650, #12225, #19616, #7005 ),
 .UNSPECIFIED., .F., .F.,
 ( 4, 2, 2, 2, 2, 2, 2, 4 ),
 ( 0.000000000000000000, 0.2500000000000000555, 0.3750000000000001110, 0.5000000000000001110, 0.6250000000000001110, 0.7500000000000000000, 0.8750000000000000000, 1.000000000000000000 ),
 .UNSPECIFIED. ) ;
#23944 = CARTESIAN_POINT ( 'NONE',  ( -4.229965536171357066, 12.22545598775685072, -2.353907750527997056 ) ) ;
#23945 = DIRECTION ( 'NONE',  ( 1.000000000000000000, 0.000000000000000000, 0.000000000000000000 ) ) ;
#23946 = CONICAL_SURFACE ( 'NONE', #20093, 2.249999993279999888, 0.7853981633972997312 ) ;
#23947 = FACE_OUTER_BOUND ( 'NONE', #8614, .T. ) ;
#23948 = VERTEX_POINT ( 'NONE', #16107 ) ;
#23949 = DIRECTION ( 'NONE',  ( 0.000000000000000000, 1.000000000000000000, 0.000000000000000000 ) ) ;
#23950 = CARTESIAN_POINT ( 'NONE',  ( 12.98081408531000136, 6.028018288394999757, 8.144720004203000130 ) ) ;
#23951 = CARTESIAN_POINT ( 'NONE',  ( 18.81919638685927865, 6.056488561384143487, 8.493049548664323822 ) ) ;
#23952 = AXIS2_PLACEMENT_3D ( 'NONE', #2316, #16723, #3903 ) ;
#23953 = CARTESIAN_POINT ( 'NONE',  ( 0.000000000000000000, 15.09999999999999964, -3.000000000000416112 ) ) ;
#23954 = CARTESIAN_POINT ( 'NONE',  ( 1.543604752742000041, 28.94076659806999885, 1.761054684240999979 ) ) ;
#23955 = DIRECTION ( 'NONE',  ( 1.000000000000000000, 0.000000000000000000, 0.000000000000000000 ) ) ;
#23956 = DIRECTION ( 'NONE',  ( 0.000000000000000000, -1.000000000000000000, 0.000000000000000000 ) ) ;
#23957 = AXIS2_PLACEMENT_3D ( 'NONE', #1213, #16089, #1088 ) ;
#23958 = ORIENTED_EDGE ( 'NONE', *, *, #17854, .T. ) ;
#23959 = AXIS2_PLACEMENT_3D ( 'NONE', #21599, #13956, #17724 ) ;
#23960 = CARTESIAN_POINT ( 'NONE',  ( -2.184465970885638431, 28.86666666666667069, 1.259047450927259559 ) ) ;
#23961 = CARTESIAN_POINT ( 'NONE',  ( 19.59345391583999785, -8.694423010569000354, -7.125817356098999689 ) ) ;
#23962 = CARTESIAN_POINT ( 'NONE',  ( -24.29403582007070739, 10.10213813269781014, -1.507518411738413944 ) ) ;
#23963 = DIRECTION ( 'NONE',  ( 0.000000000000000000, 1.000000000000000000, 0.000000000000000000 ) ) ;
#23964 = CYLINDRICAL_SURFACE ( 'NONE', #15693, 15.45000000000000107 ) ;
#23965 = CARTESIAN_POINT ( 'NONE',  ( -1.099784704884000375, 11.50157083293000504, 4.823590451572001392 ) ) ;
#23966 = CARTESIAN_POINT ( 'NONE',  ( -1.033211977243992497, 29.26718191722662965, -1.899078110007318188 ) ) ;
#23967 = LINE ( 'NONE', #9199, #2283 ) ;
#23968 = CARTESIAN_POINT ( 'NONE',  ( 17.94318924931000225, -0.08898103000111000360, -10.77198407497000154 ) ) ;
#23969 = NEXT_ASSEMBLY_USAGE_OCCURRENCE ( 'NAUO1', ' ', ' ', #6191, #1482, $ ) ;
#23970 = NEXT_ASSEMBLY_USAGE_OCCURRENCE ( 'NAUO2', ' ', ' ', #6191, #5757, $ ) ;
#23971 = NEXT_ASSEMBLY_USAGE_OCCURRENCE ( 'NAUO3', ' ', ' ', #6191, #2198, $ ) ;
#23972 = NEXT_ASSEMBLY_USAGE_OCCURRENCE ( 'NAUO4', ' ', ' ', #6191, #116, $ ) ;
#23973 = NEXT_ASSEMBLY_USAGE_OCCURRENCE ( 'NAUO5', ' ', ' ', #6191, #2646, $ ) ;
#23974 = NEXT_ASSEMBLY_USAGE_OCCURRENCE ( 'NAUO6', ' ', ' ', #6191, #8728, $ ) ;
#23975 = NEXT_ASSEMBLY_USAGE_OCCURRENCE ( 'NAUO7', ' ', ' ', #6191, #116, $ ) ;
ENDSEC;
END-ISO-10303-21;
